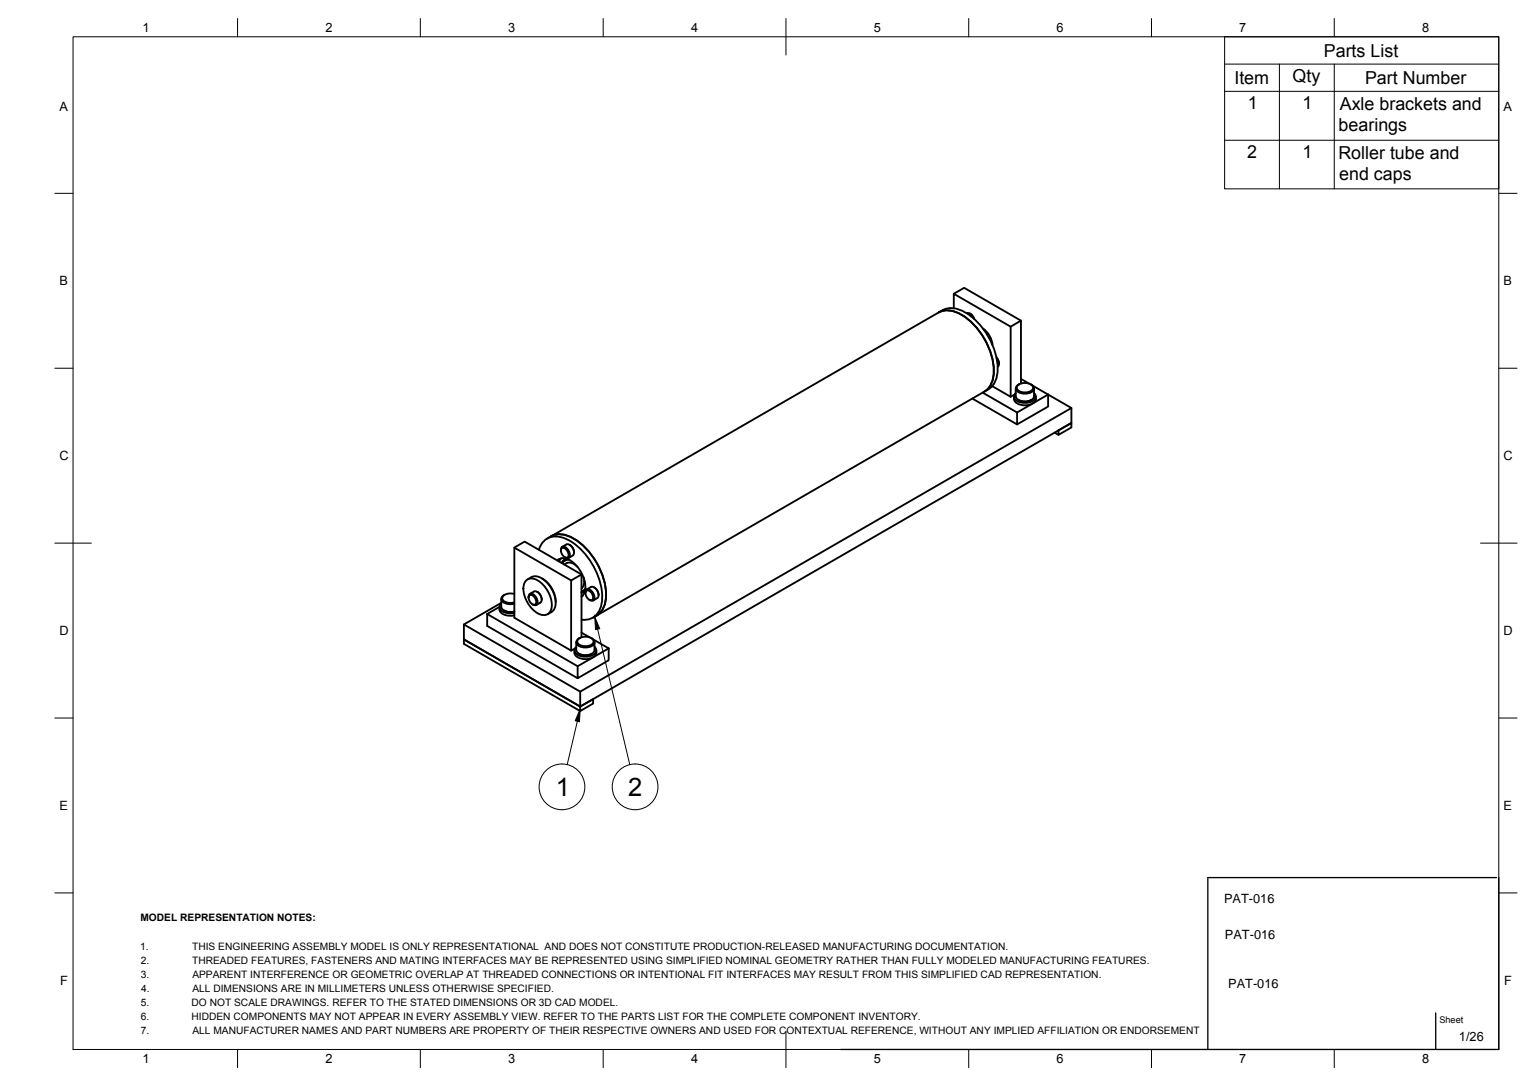
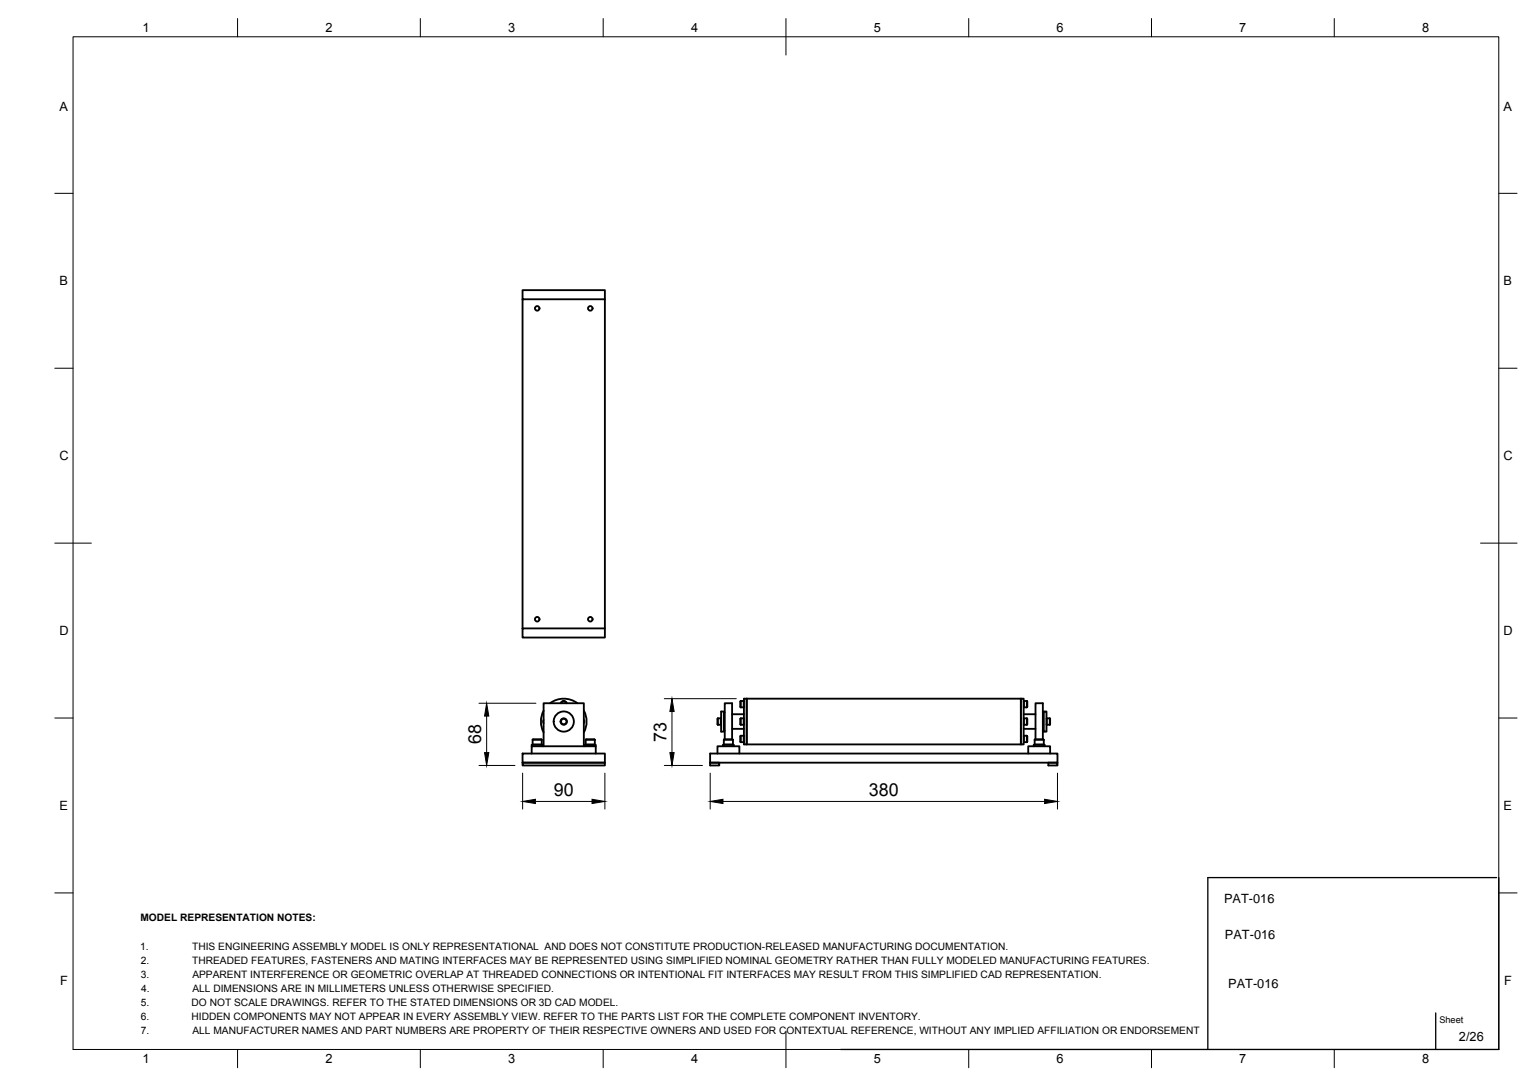
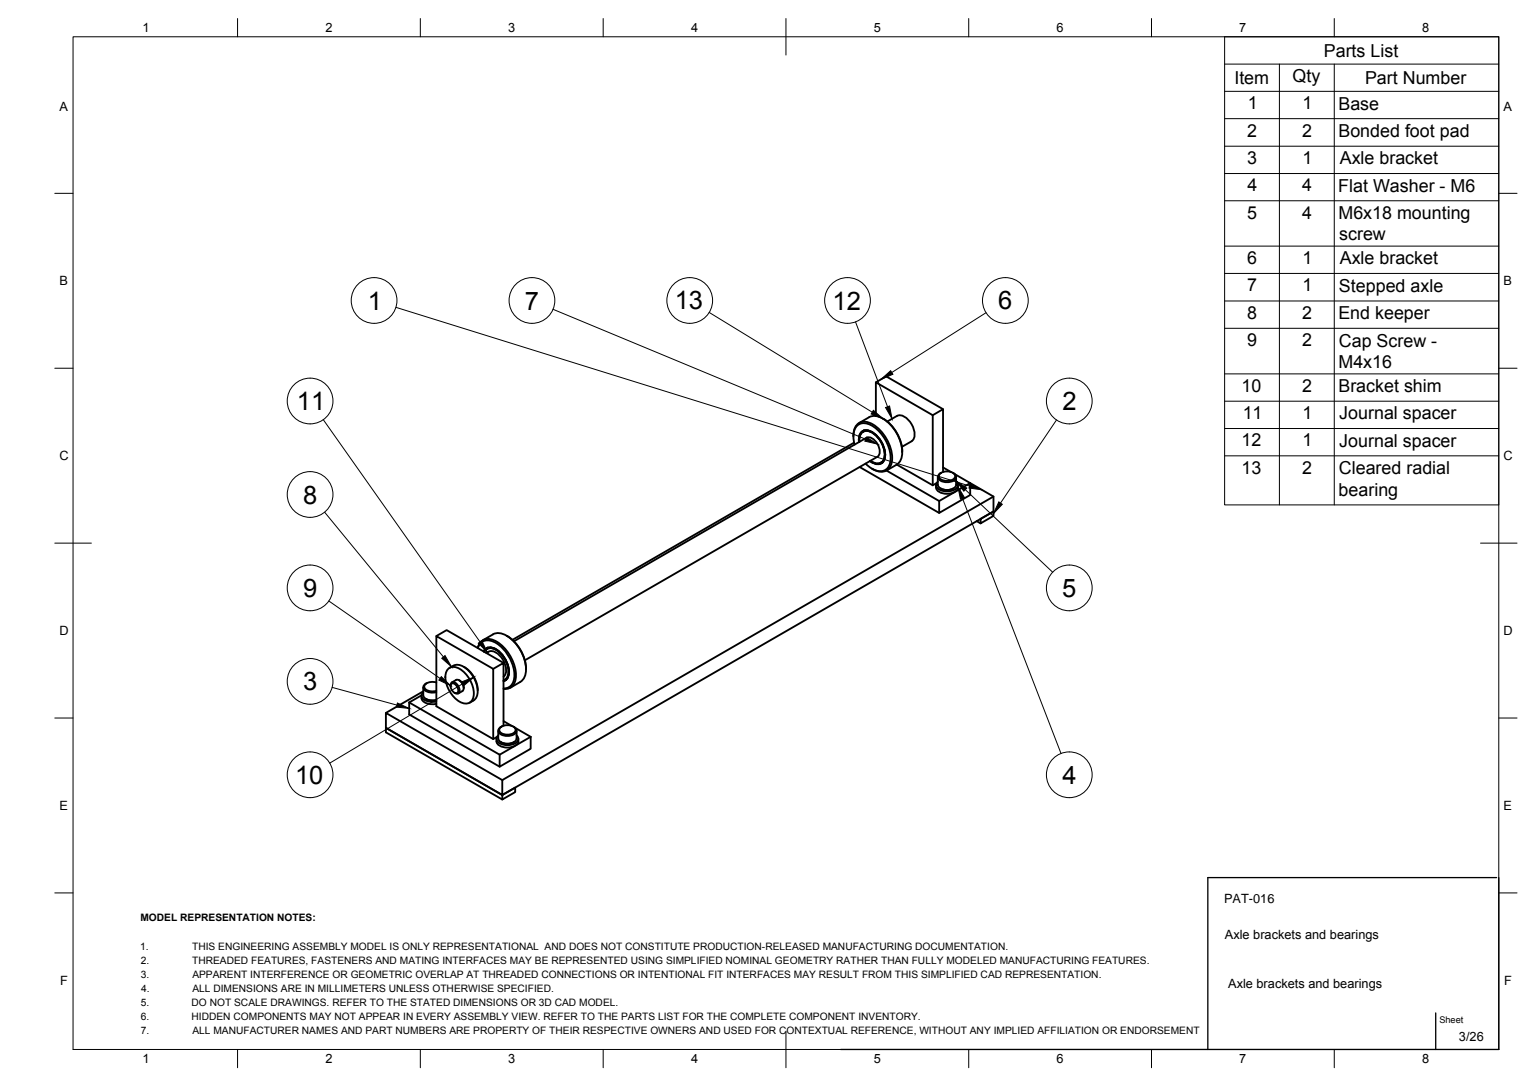
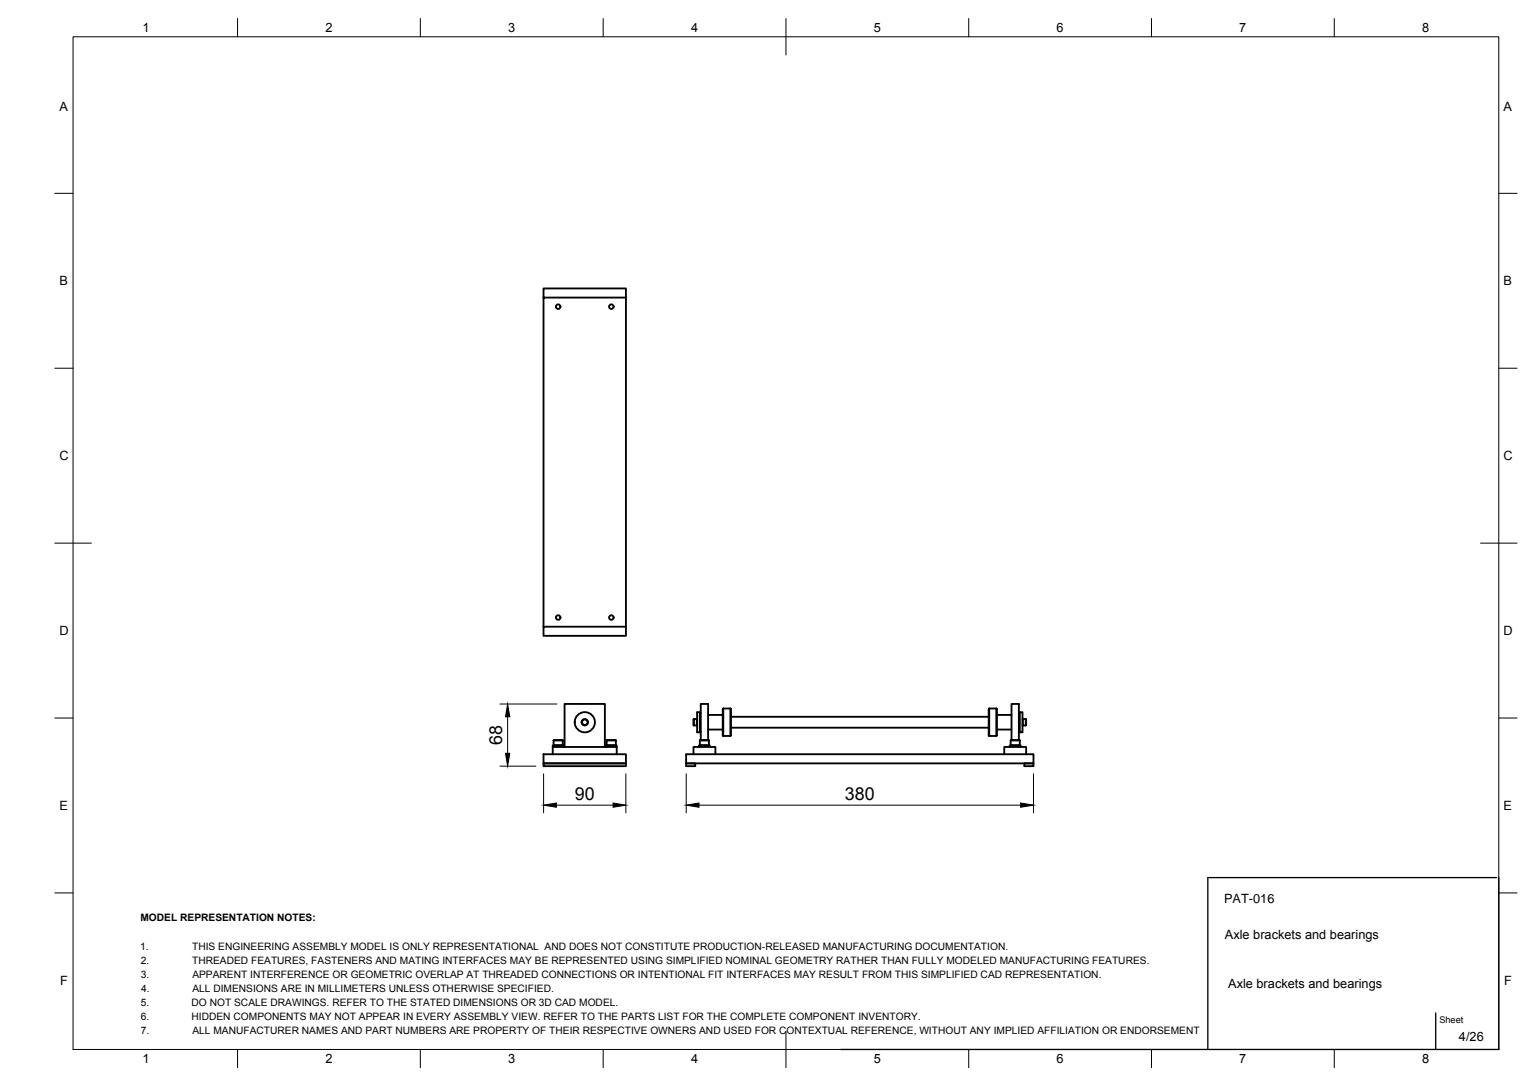
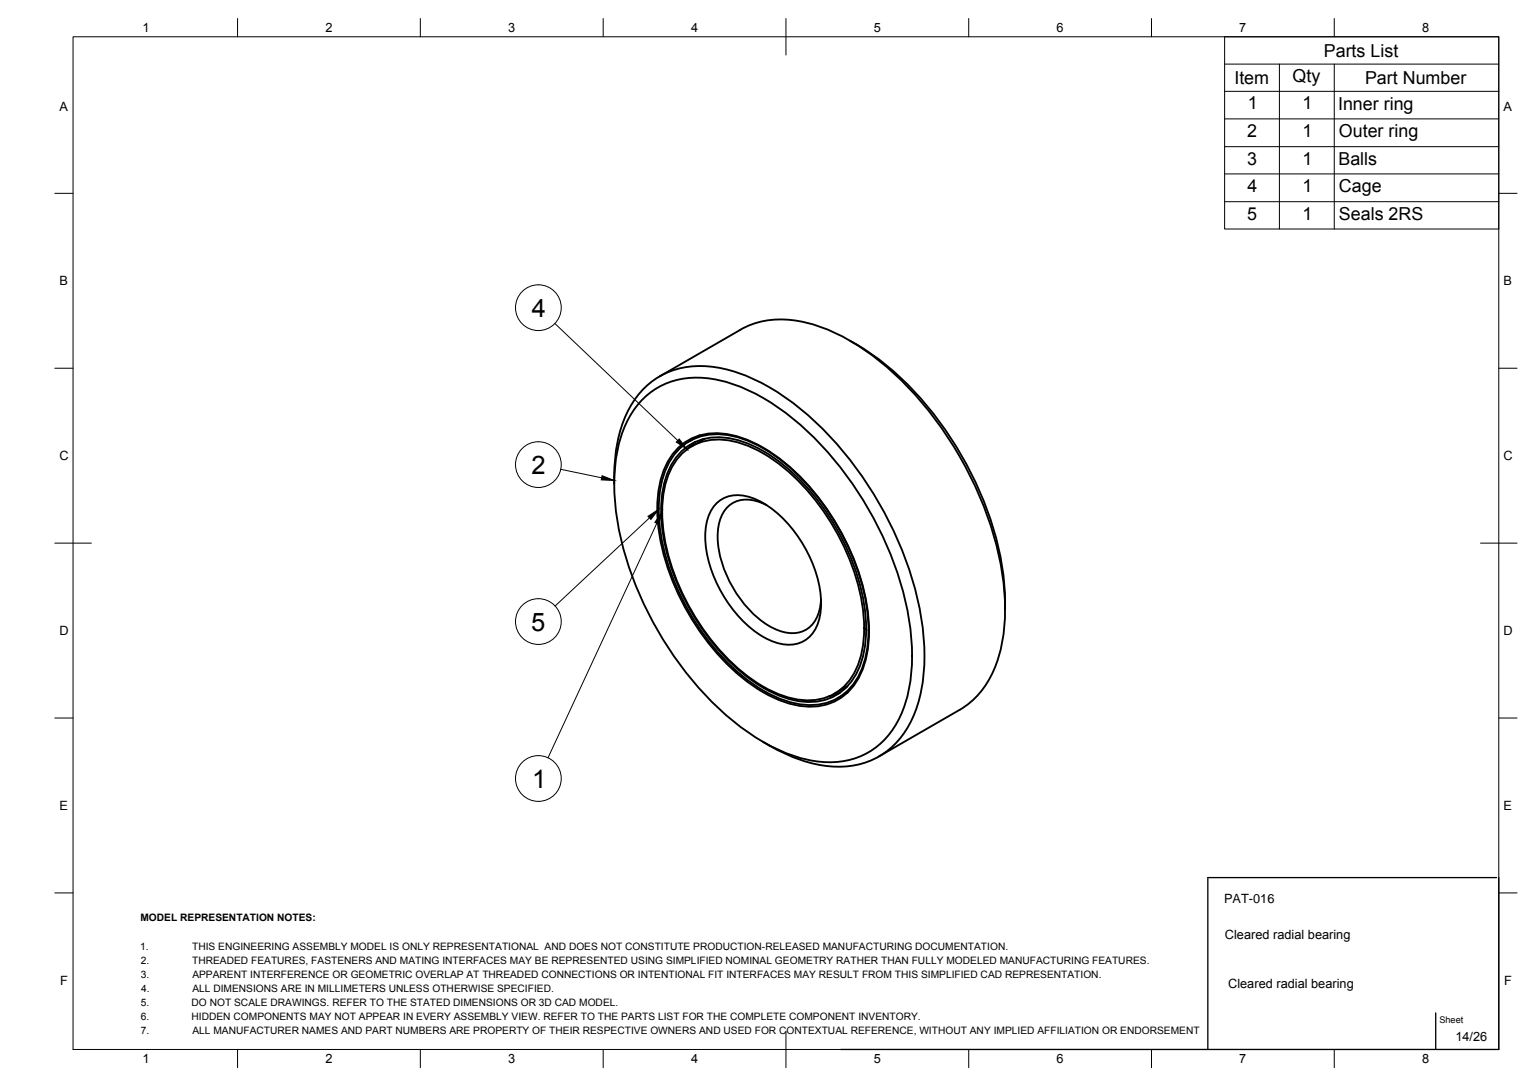
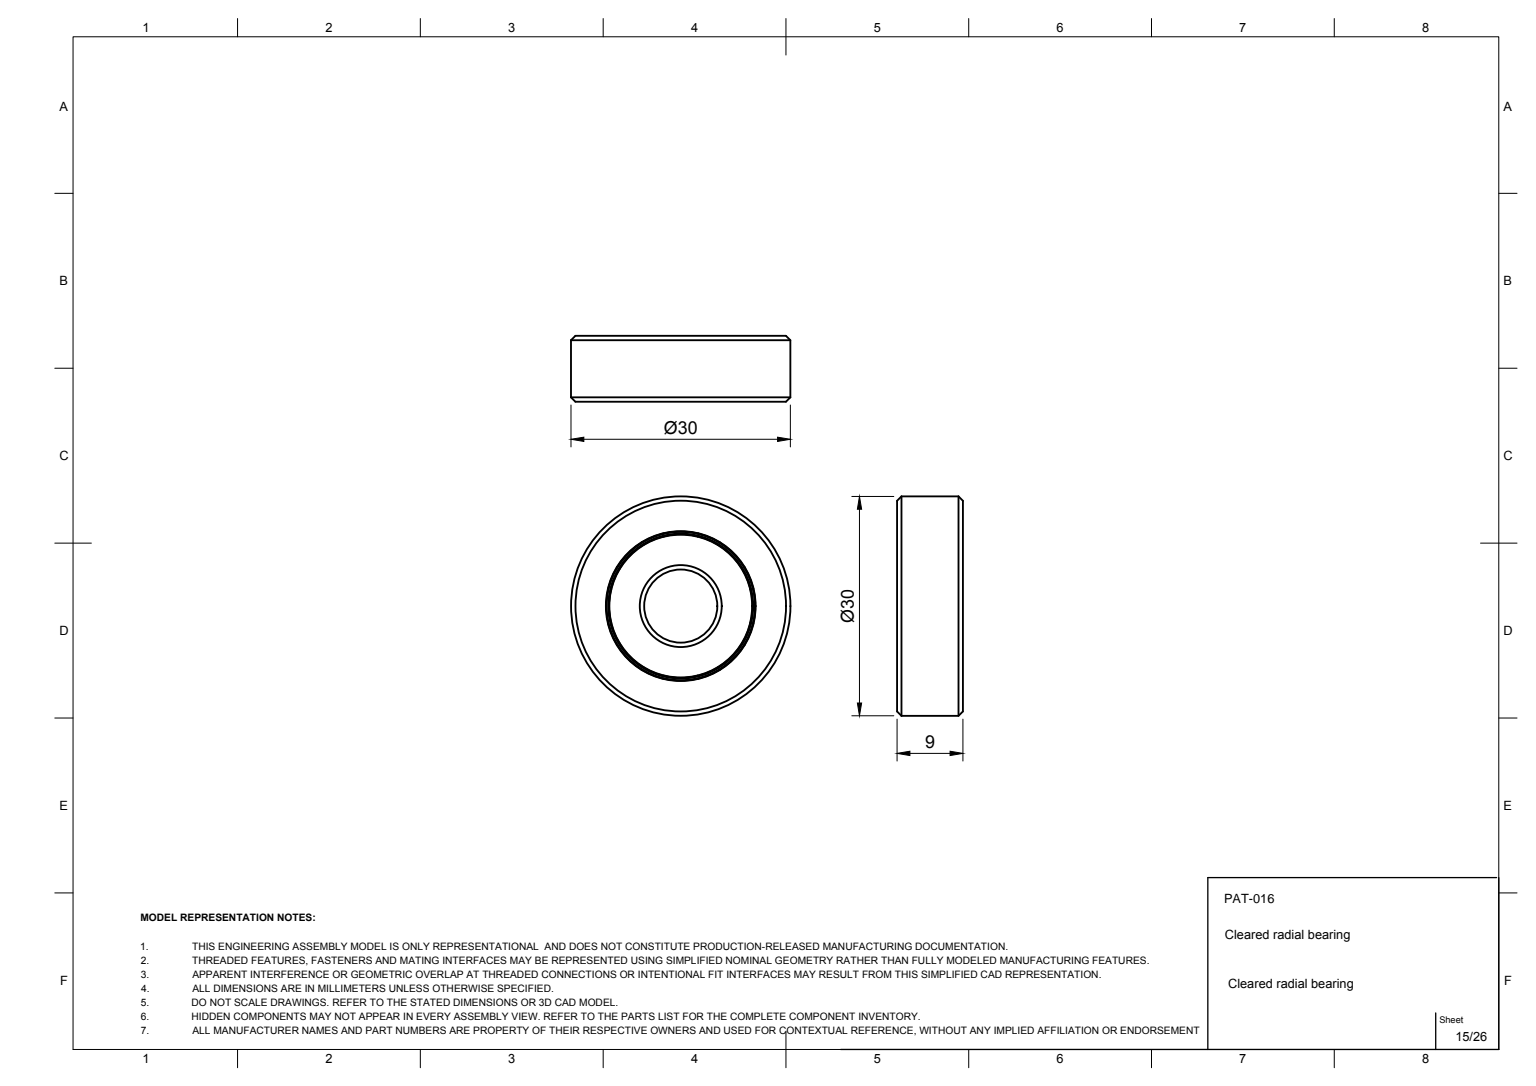
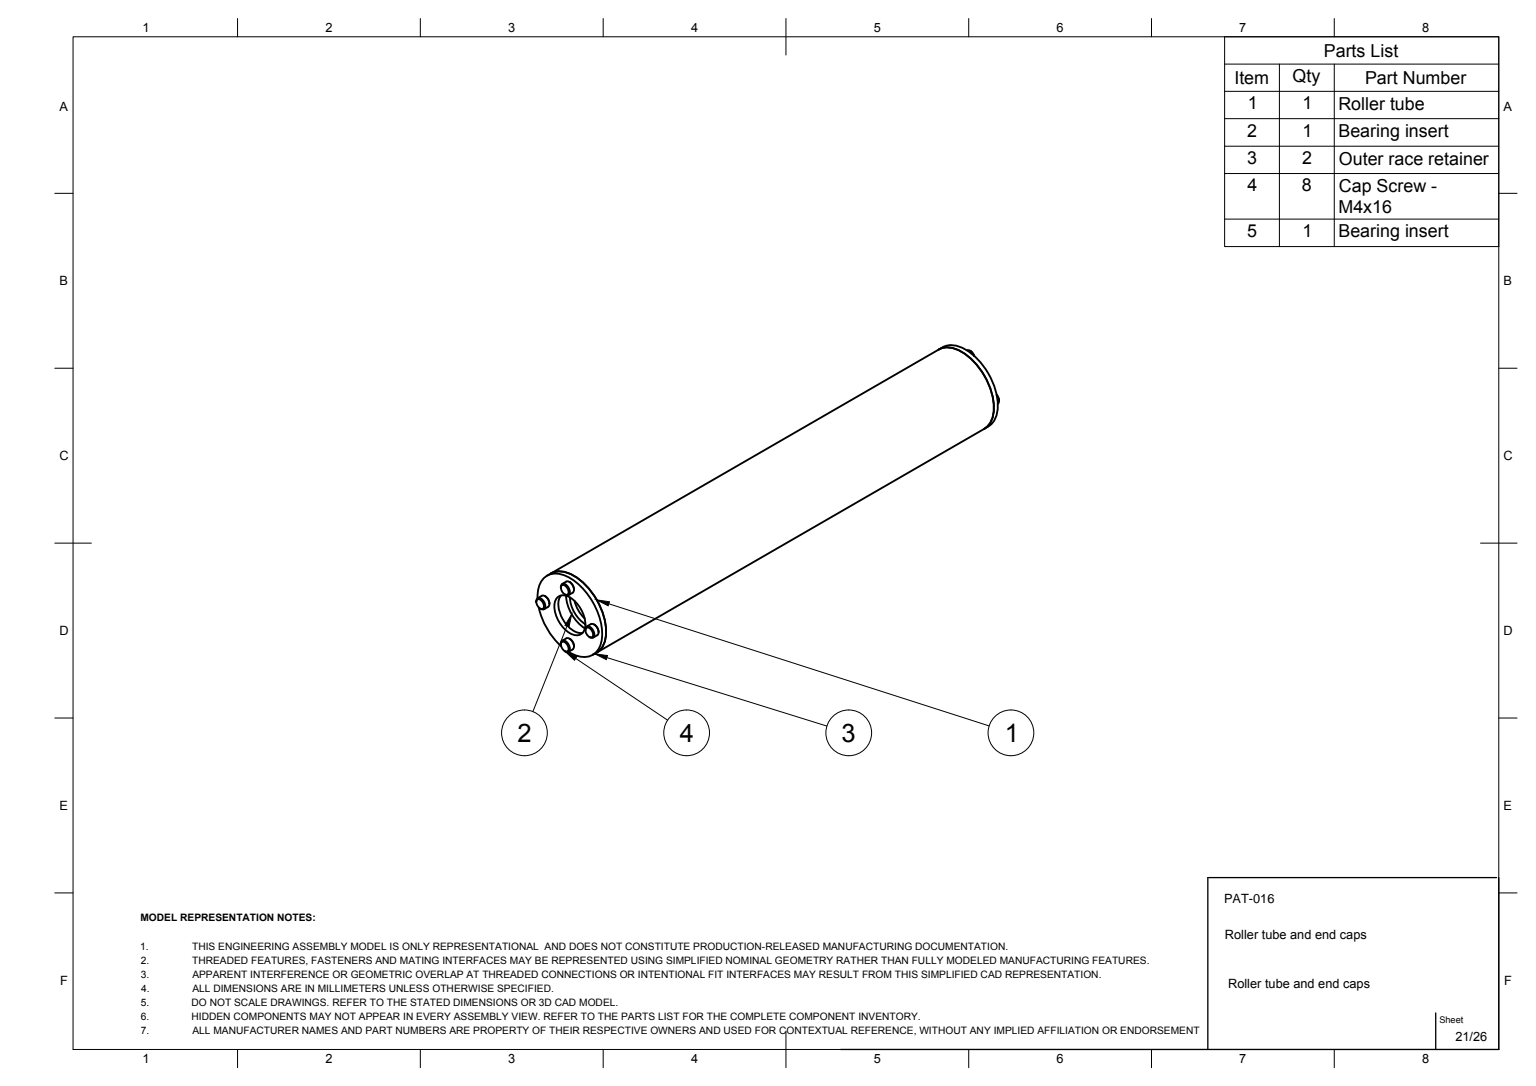
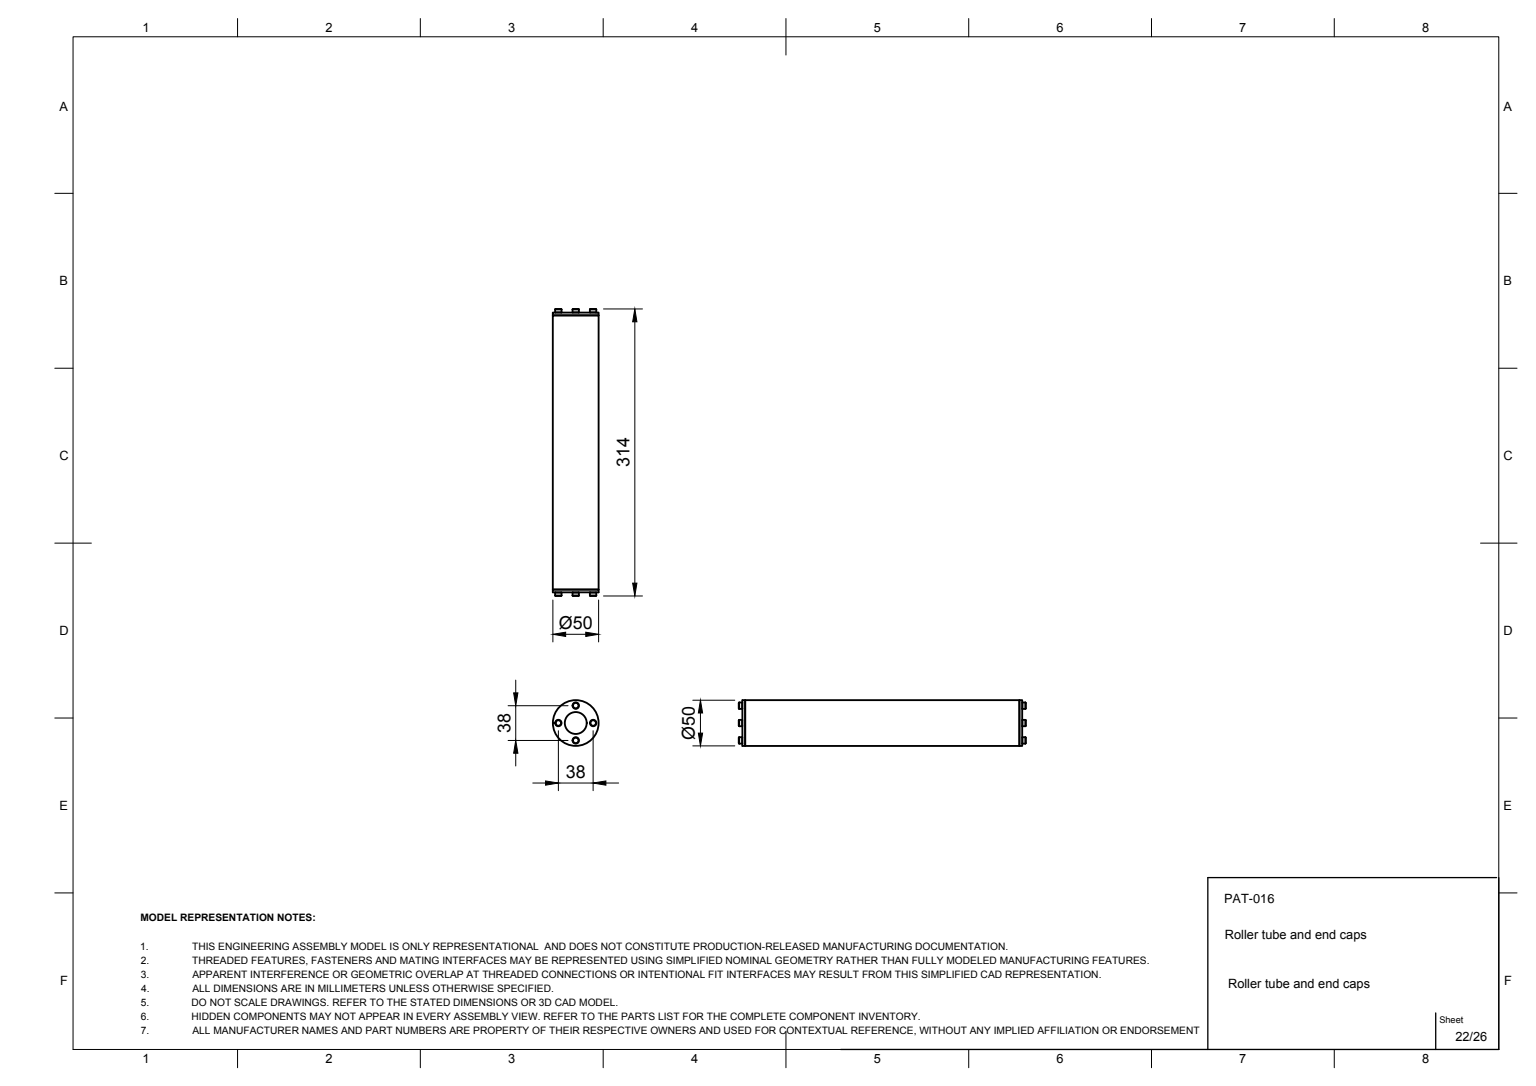
ISO-10303-21;
HEADER;
/* Generated by software containing ST-Developer
 * from STEP Tools, Inc. (www.steptools.com) 
 */

FILE_DESCRIPTION(
/* description */ ('Bracket-mounted idler roller'),
/* implementation_level */ '2;1');

FILE_NAME(
/* name */ 'PAT-016',
/* time_stamp */ '2026-10-28T03:26:42-07:00',
/* author */ (''),
/* organization */ (''),
/* preprocessor_version */ 'ST-DEVELOPER v20.2',
/* originating_system */ 'Autodesk Translation Framework v15.17.0.0',
/* authorisation */ '');

FILE_SCHEMA (('AUTOMOTIVE_DESIGN { 1 0 10303 214 3 1 1 }'));
ENDSEC;

DATA;
#10=MECHANICAL_DESIGN_GEOMETRIC_PRESENTATION_REPRESENTATION('',(#280,#281,
#282,#283,#284,#285,#286,#287,#288,#289,#290,#291,#292,#293,#294,#295,#296,
#297,#298,#299,#300,#301,#302,#303,#304,#305,#306,#307,#308),#6241);
#11=ITEM_DEFINED_TRANSFORMATION($,$,#3607,#3735);
#12=ITEM_DEFINED_TRANSFORMATION($,$,#3627,#3736);
#13=ITEM_DEFINED_TRANSFORMATION($,$,#3647,#3737);
#14=ITEM_DEFINED_TRANSFORMATION($,$,#3664,#3738);
#15=ITEM_DEFINED_TRANSFORMATION($,$,#3718,#3739);
#16=ITEM_DEFINED_TRANSFORMATION($,$,#3447,#3847);
#17=ITEM_DEFINED_TRANSFORMATION($,$,#3468,#3848);
#18=ITEM_DEFINED_TRANSFORMATION($,$,#3489,#3849);
#19=ITEM_DEFINED_TRANSFORMATION($,$,#3511,#3850);
#20=ITEM_DEFINED_TRANSFORMATION($,$,#3520,#3851);
#21=ITEM_DEFINED_TRANSFORMATION($,$,#3529,#3852);
#22=ITEM_DEFINED_TRANSFORMATION($,$,#3548,#3853);
#23=ITEM_DEFINED_TRANSFORMATION($,$,#3548,#3854);
#24=ITEM_DEFINED_TRANSFORMATION($,$,#3555,#3855);
#25=ITEM_DEFINED_TRANSFORMATION($,$,#3564,#3856);
#26=ITEM_DEFINED_TRANSFORMATION($,$,#3555,#3857);
#27=ITEM_DEFINED_TRANSFORMATION($,$,#3564,#3858);
#28=ITEM_DEFINED_TRANSFORMATION($,$,#3555,#3859);
#29=ITEM_DEFINED_TRANSFORMATION($,$,#3564,#3860);
#30=ITEM_DEFINED_TRANSFORMATION($,$,#3555,#3861);
#31=ITEM_DEFINED_TRANSFORMATION($,$,#3564,#3862);
#32=ITEM_DEFINED_TRANSFORMATION($,$,#3588,#3863);
#33=ITEM_DEFINED_TRANSFORMATION($,$,#3588,#3864);
#34=ITEM_DEFINED_TRANSFORMATION($,$,#3821,#3865);
#35=ITEM_DEFINED_TRANSFORMATION($,$,#3821,#3866);
#36=ITEM_DEFINED_TRANSFORMATION($,$,#3597,#3867);
#37=ITEM_DEFINED_TRANSFORMATION($,$,#3597,#3868);
#38=ITEM_DEFINED_TRANSFORMATION($,$,#3606,#3869);
#39=ITEM_DEFINED_TRANSFORMATION($,$,#3606,#3870);
#40=ITEM_DEFINED_TRANSFORMATION($,$,#3741,#3871);
#41=ITEM_DEFINED_TRANSFORMATION($,$,#3766,#3872);
#42=ITEM_DEFINED_TRANSFORMATION($,$,#3791,#3873);
#43=ITEM_DEFINED_TRANSFORMATION($,$,#3800,#3874);
#44=ITEM_DEFINED_TRANSFORMATION($,$,#3821,#3875);
#45=ITEM_DEFINED_TRANSFORMATION($,$,#3821,#3876);
#46=ITEM_DEFINED_TRANSFORMATION($,$,#3821,#3877);
#47=ITEM_DEFINED_TRANSFORMATION($,$,#3821,#3878);
#48=ITEM_DEFINED_TRANSFORMATION($,$,#3800,#3879);
#49=ITEM_DEFINED_TRANSFORMATION($,$,#3821,#3880);
#50=ITEM_DEFINED_TRANSFORMATION($,$,#3821,#3881);
#51=ITEM_DEFINED_TRANSFORMATION($,$,#3821,#3882);
#52=ITEM_DEFINED_TRANSFORMATION($,$,#3821,#3883);
#53=ITEM_DEFINED_TRANSFORMATION($,$,#3446,#3884);
#54=ITEM_DEFINED_TRANSFORMATION($,$,#3740,#3885);
#55=(
REPRESENTATION_RELATIONSHIP($,$,#6354,#6353)
REPRESENTATION_RELATIONSHIP_WITH_TRANSFORMATION(#11)
SHAPE_REPRESENTATION_RELATIONSHIP()
);
#56=(
REPRESENTATION_RELATIONSHIP($,$,#6355,#6353)
REPRESENTATION_RELATIONSHIP_WITH_TRANSFORMATION(#12)
SHAPE_REPRESENTATION_RELATIONSHIP()
);
#57=(
REPRESENTATION_RELATIONSHIP($,$,#6356,#6353)
REPRESENTATION_RELATIONSHIP_WITH_TRANSFORMATION(#13)
SHAPE_REPRESENTATION_RELATIONSHIP()
);
#58=(
REPRESENTATION_RELATIONSHIP($,$,#6357,#6353)
REPRESENTATION_RELATIONSHIP_WITH_TRANSFORMATION(#14)
SHAPE_REPRESENTATION_RELATIONSHIP()
);
#59=(
REPRESENTATION_RELATIONSHIP($,$,#6358,#6353)
REPRESENTATION_RELATIONSHIP_WITH_TRANSFORMATION(#15)
SHAPE_REPRESENTATION_RELATIONSHIP()
);
#60=(
REPRESENTATION_RELATIONSHIP($,$,#6342,#6341)
REPRESENTATION_RELATIONSHIP_WITH_TRANSFORMATION(#16)
SHAPE_REPRESENTATION_RELATIONSHIP()
);
#61=(
REPRESENTATION_RELATIONSHIP($,$,#6343,#6341)
REPRESENTATION_RELATIONSHIP_WITH_TRANSFORMATION(#17)
SHAPE_REPRESENTATION_RELATIONSHIP()
);
#62=(
REPRESENTATION_RELATIONSHIP($,$,#6344,#6341)
REPRESENTATION_RELATIONSHIP_WITH_TRANSFORMATION(#18)
SHAPE_REPRESENTATION_RELATIONSHIP()
);
#63=(
REPRESENTATION_RELATIONSHIP($,$,#6345,#6341)
REPRESENTATION_RELATIONSHIP_WITH_TRANSFORMATION(#19)
SHAPE_REPRESENTATION_RELATIONSHIP()
);
#64=(
REPRESENTATION_RELATIONSHIP($,$,#6346,#6341)
REPRESENTATION_RELATIONSHIP_WITH_TRANSFORMATION(#20)
SHAPE_REPRESENTATION_RELATIONSHIP()
);
#65=(
REPRESENTATION_RELATIONSHIP($,$,#6347,#6341)
REPRESENTATION_RELATIONSHIP_WITH_TRANSFORMATION(#21)
SHAPE_REPRESENTATION_RELATIONSHIP()
);
#66=(
REPRESENTATION_RELATIONSHIP($,$,#6348,#6341)
REPRESENTATION_RELATIONSHIP_WITH_TRANSFORMATION(#22)
SHAPE_REPRESENTATION_RELATIONSHIP()
);
#67=(
REPRESENTATION_RELATIONSHIP($,$,#6348,#6341)
REPRESENTATION_RELATIONSHIP_WITH_TRANSFORMATION(#23)
SHAPE_REPRESENTATION_RELATIONSHIP()
);
#68=(
REPRESENTATION_RELATIONSHIP($,$,#6349,#6341)
REPRESENTATION_RELATIONSHIP_WITH_TRANSFORMATION(#24)
SHAPE_REPRESENTATION_RELATIONSHIP()
);
#69=(
REPRESENTATION_RELATIONSHIP($,$,#6350,#6341)
REPRESENTATION_RELATIONSHIP_WITH_TRANSFORMATION(#25)
SHAPE_REPRESENTATION_RELATIONSHIP()
);
#70=(
REPRESENTATION_RELATIONSHIP($,$,#6349,#6341)
REPRESENTATION_RELATIONSHIP_WITH_TRANSFORMATION(#26)
SHAPE_REPRESENTATION_RELATIONSHIP()
);
#71=(
REPRESENTATION_RELATIONSHIP($,$,#6350,#6341)
REPRESENTATION_RELATIONSHIP_WITH_TRANSFORMATION(#27)
SHAPE_REPRESENTATION_RELATIONSHIP()
);
#72=(
REPRESENTATION_RELATIONSHIP($,$,#6349,#6341)
REPRESENTATION_RELATIONSHIP_WITH_TRANSFORMATION(#28)
SHAPE_REPRESENTATION_RELATIONSHIP()
);
#73=(
REPRESENTATION_RELATIONSHIP($,$,#6350,#6341)
REPRESENTATION_RELATIONSHIP_WITH_TRANSFORMATION(#29)
SHAPE_REPRESENTATION_RELATIONSHIP()
);
#74=(
REPRESENTATION_RELATIONSHIP($,$,#6349,#6341)
REPRESENTATION_RELATIONSHIP_WITH_TRANSFORMATION(#30)
SHAPE_REPRESENTATION_RELATIONSHIP()
);
#75=(
REPRESENTATION_RELATIONSHIP($,$,#6350,#6341)
REPRESENTATION_RELATIONSHIP_WITH_TRANSFORMATION(#31)
SHAPE_REPRESENTATION_RELATIONSHIP()
);
#76=(
REPRESENTATION_RELATIONSHIP($,$,#6351,#6341)
REPRESENTATION_RELATIONSHIP_WITH_TRANSFORMATION(#32)
SHAPE_REPRESENTATION_RELATIONSHIP()
);
#77=(
REPRESENTATION_RELATIONSHIP($,$,#6351,#6341)
REPRESENTATION_RELATIONSHIP_WITH_TRANSFORMATION(#33)
SHAPE_REPRESENTATION_RELATIONSHIP()
);
#78=(
REPRESENTATION_RELATIONSHIP($,$,#6364,#6341)
REPRESENTATION_RELATIONSHIP_WITH_TRANSFORMATION(#34)
SHAPE_REPRESENTATION_RELATIONSHIP()
);
#79=(
REPRESENTATION_RELATIONSHIP($,$,#6364,#6341)
REPRESENTATION_RELATIONSHIP_WITH_TRANSFORMATION(#35)
SHAPE_REPRESENTATION_RELATIONSHIP()
);
#80=(
REPRESENTATION_RELATIONSHIP($,$,#6352,#6341)
REPRESENTATION_RELATIONSHIP_WITH_TRANSFORMATION(#36)
SHAPE_REPRESENTATION_RELATIONSHIP()
);
#81=(
REPRESENTATION_RELATIONSHIP($,$,#6352,#6341)
REPRESENTATION_RELATIONSHIP_WITH_TRANSFORMATION(#37)
SHAPE_REPRESENTATION_RELATIONSHIP()
);
#82=(
REPRESENTATION_RELATIONSHIP($,$,#6353,#6341)
REPRESENTATION_RELATIONSHIP_WITH_TRANSFORMATION(#38)
SHAPE_REPRESENTATION_RELATIONSHIP()
);
#83=(
REPRESENTATION_RELATIONSHIP($,$,#6353,#6341)
REPRESENTATION_RELATIONSHIP_WITH_TRANSFORMATION(#39)
SHAPE_REPRESENTATION_RELATIONSHIP()
);
#84=(
REPRESENTATION_RELATIONSHIP($,$,#6360,#6359)
REPRESENTATION_RELATIONSHIP_WITH_TRANSFORMATION(#40)
SHAPE_REPRESENTATION_RELATIONSHIP()
);
#85=(
REPRESENTATION_RELATIONSHIP($,$,#6361,#6359)
REPRESENTATION_RELATIONSHIP_WITH_TRANSFORMATION(#41)
SHAPE_REPRESENTATION_RELATIONSHIP()
);
#86=(
REPRESENTATION_RELATIONSHIP($,$,#6362,#6359)
REPRESENTATION_RELATIONSHIP_WITH_TRANSFORMATION(#42)
SHAPE_REPRESENTATION_RELATIONSHIP()
);
#87=(
REPRESENTATION_RELATIONSHIP($,$,#6363,#6359)
REPRESENTATION_RELATIONSHIP_WITH_TRANSFORMATION(#43)
SHAPE_REPRESENTATION_RELATIONSHIP()
);
#88=(
REPRESENTATION_RELATIONSHIP($,$,#6364,#6359)
REPRESENTATION_RELATIONSHIP_WITH_TRANSFORMATION(#44)
SHAPE_REPRESENTATION_RELATIONSHIP()
);
#89=(
REPRESENTATION_RELATIONSHIP($,$,#6364,#6359)
REPRESENTATION_RELATIONSHIP_WITH_TRANSFORMATION(#45)
SHAPE_REPRESENTATION_RELATIONSHIP()
);
#90=(
REPRESENTATION_RELATIONSHIP($,$,#6364,#6359)
REPRESENTATION_RELATIONSHIP_WITH_TRANSFORMATION(#46)
SHAPE_REPRESENTATION_RELATIONSHIP()
);
#91=(
REPRESENTATION_RELATIONSHIP($,$,#6364,#6359)
REPRESENTATION_RELATIONSHIP_WITH_TRANSFORMATION(#47)
SHAPE_REPRESENTATION_RELATIONSHIP()
);
#92=(
REPRESENTATION_RELATIONSHIP($,$,#6363,#6359)
REPRESENTATION_RELATIONSHIP_WITH_TRANSFORMATION(#48)
SHAPE_REPRESENTATION_RELATIONSHIP()
);
#93=(
REPRESENTATION_RELATIONSHIP($,$,#6364,#6359)
REPRESENTATION_RELATIONSHIP_WITH_TRANSFORMATION(#49)
SHAPE_REPRESENTATION_RELATIONSHIP()
);
#94=(
REPRESENTATION_RELATIONSHIP($,$,#6364,#6359)
REPRESENTATION_RELATIONSHIP_WITH_TRANSFORMATION(#50)
SHAPE_REPRESENTATION_RELATIONSHIP()
);
#95=(
REPRESENTATION_RELATIONSHIP($,$,#6364,#6359)
REPRESENTATION_RELATIONSHIP_WITH_TRANSFORMATION(#51)
SHAPE_REPRESENTATION_RELATIONSHIP()
);
#96=(
REPRESENTATION_RELATIONSHIP($,$,#6364,#6359)
REPRESENTATION_RELATIONSHIP_WITH_TRANSFORMATION(#52)
SHAPE_REPRESENTATION_RELATIONSHIP()
);
#97=(
REPRESENTATION_RELATIONSHIP($,$,#6341,#6340)
REPRESENTATION_RELATIONSHIP_WITH_TRANSFORMATION(#53)
SHAPE_REPRESENTATION_RELATIONSHIP()
);
#98=(
REPRESENTATION_RELATIONSHIP($,$,#6359,#6340)
REPRESENTATION_RELATIONSHIP_WITH_TRANSFORMATION(#54)
SHAPE_REPRESENTATION_RELATIONSHIP()
);
#99=CONTEXT_DEPENDENT_SHAPE_REPRESENTATION(#55,#6290);
#100=CONTEXT_DEPENDENT_SHAPE_REPRESENTATION(#56,#6291);
#101=CONTEXT_DEPENDENT_SHAPE_REPRESENTATION(#57,#6292);
#102=CONTEXT_DEPENDENT_SHAPE_REPRESENTATION(#58,#6293);
#103=CONTEXT_DEPENDENT_SHAPE_REPRESENTATION(#59,#6294);
#104=CONTEXT_DEPENDENT_SHAPE_REPRESENTATION(#60,#6301);
#105=CONTEXT_DEPENDENT_SHAPE_REPRESENTATION(#61,#6302);
#106=CONTEXT_DEPENDENT_SHAPE_REPRESENTATION(#62,#6303);
#107=CONTEXT_DEPENDENT_SHAPE_REPRESENTATION(#63,#6304);
#108=CONTEXT_DEPENDENT_SHAPE_REPRESENTATION(#64,#6305);
#109=CONTEXT_DEPENDENT_SHAPE_REPRESENTATION(#65,#6306);
#110=CONTEXT_DEPENDENT_SHAPE_REPRESENTATION(#66,#6307);
#111=CONTEXT_DEPENDENT_SHAPE_REPRESENTATION(#67,#6308);
#112=CONTEXT_DEPENDENT_SHAPE_REPRESENTATION(#68,#6309);
#113=CONTEXT_DEPENDENT_SHAPE_REPRESENTATION(#69,#6310);
#114=CONTEXT_DEPENDENT_SHAPE_REPRESENTATION(#70,#6311);
#115=CONTEXT_DEPENDENT_SHAPE_REPRESENTATION(#71,#6312);
#116=CONTEXT_DEPENDENT_SHAPE_REPRESENTATION(#72,#6313);
#117=CONTEXT_DEPENDENT_SHAPE_REPRESENTATION(#73,#6314);
#118=CONTEXT_DEPENDENT_SHAPE_REPRESENTATION(#74,#6315);
#119=CONTEXT_DEPENDENT_SHAPE_REPRESENTATION(#75,#6316);
#120=CONTEXT_DEPENDENT_SHAPE_REPRESENTATION(#76,#6317);
#121=CONTEXT_DEPENDENT_SHAPE_REPRESENTATION(#77,#6318);
#122=CONTEXT_DEPENDENT_SHAPE_REPRESENTATION(#78,#6319);
#123=CONTEXT_DEPENDENT_SHAPE_REPRESENTATION(#79,#6320);
#124=CONTEXT_DEPENDENT_SHAPE_REPRESENTATION(#80,#6321);
#125=CONTEXT_DEPENDENT_SHAPE_REPRESENTATION(#81,#6322);
#126=CONTEXT_DEPENDENT_SHAPE_REPRESENTATION(#82,#6323);
#127=CONTEXT_DEPENDENT_SHAPE_REPRESENTATION(#83,#6324);
#128=CONTEXT_DEPENDENT_SHAPE_REPRESENTATION(#84,#6325);
#129=CONTEXT_DEPENDENT_SHAPE_REPRESENTATION(#85,#6326);
#130=CONTEXT_DEPENDENT_SHAPE_REPRESENTATION(#86,#6327);
#131=CONTEXT_DEPENDENT_SHAPE_REPRESENTATION(#87,#6328);
#132=CONTEXT_DEPENDENT_SHAPE_REPRESENTATION(#88,#6329);
#133=CONTEXT_DEPENDENT_SHAPE_REPRESENTATION(#89,#6330);
#134=CONTEXT_DEPENDENT_SHAPE_REPRESENTATION(#90,#6331);
#135=CONTEXT_DEPENDENT_SHAPE_REPRESENTATION(#91,#6332);
#136=CONTEXT_DEPENDENT_SHAPE_REPRESENTATION(#92,#6333);
#137=CONTEXT_DEPENDENT_SHAPE_REPRESENTATION(#93,#6334);
#138=CONTEXT_DEPENDENT_SHAPE_REPRESENTATION(#94,#6335);
#139=CONTEXT_DEPENDENT_SHAPE_REPRESENTATION(#95,#6336);
#140=CONTEXT_DEPENDENT_SHAPE_REPRESENTATION(#96,#6337);
#141=CONTEXT_DEPENDENT_SHAPE_REPRESENTATION(#97,#6338);
#142=CONTEXT_DEPENDENT_SHAPE_REPRESENTATION(#98,#6339);
#143=NEXT_ASSEMBLY_USAGE_OCCURRENCE('Inner ring:1','Inner ring:1',
'Inner ring:1',#6379,#6380,'Inner ring:1');
#144=NEXT_ASSEMBLY_USAGE_OCCURRENCE('Outer ring:1','Outer ring:1',
'Outer ring:1',#6379,#6381,'Outer ring:1');
#145=NEXT_ASSEMBLY_USAGE_OCCURRENCE('Balls:1','Balls:1','Balls:1',#6379,
#6382,'Balls:1');
#146=NEXT_ASSEMBLY_USAGE_OCCURRENCE('Cage:1','Cage:1','Cage:1',#6379,#6383,
'Cage:1');
#147=NEXT_ASSEMBLY_USAGE_OCCURRENCE('Seals 2RS:1','Seals 2RS:1',
'Seals 2RS:1',#6379,#6384,'Seals 2RS:1');
#148=NEXT_ASSEMBLY_USAGE_OCCURRENCE('Axle bracket:1','Axle bracket:1',
'Axle bracket:1',#6367,#6368,'Axle bracket:1');
#149=NEXT_ASSEMBLY_USAGE_OCCURRENCE('Axle bracket (1):1',
'Axle bracket (1):1','Axle bracket (1):1',#6367,#6369,
'Axle bracket (1):1');
#150=NEXT_ASSEMBLY_USAGE_OCCURRENCE('Stepped axle:1','Stepped axle:1',
'Stepped axle:1',#6367,#6370,'Stepped axle:1');
#151=NEXT_ASSEMBLY_USAGE_OCCURRENCE('Journal spacer:1',
'Journal spacer:1','Journal spacer:1',#6367,#6371,'Journal spacer:1');
#152=NEXT_ASSEMBLY_USAGE_OCCURRENCE('Journal spacer (1):1',
'Journal spacer (1):1','Journal spacer (1):1',#6367,#6372,
'Journal spacer (1):1');
#153=NEXT_ASSEMBLY_USAGE_OCCURRENCE('Base:2','Base:2','Base:2',#6367,#6373,
'Base:2');
#154=NEXT_ASSEMBLY_USAGE_OCCURRENCE('Bonded foot pad:2',
'Bonded foot pad:2','Bonded foot pad:2',#6367,#6374,'Bonded foot pad:2');
#155=NEXT_ASSEMBLY_USAGE_OCCURRENCE('Bonded foot pad:3',
'Bonded foot pad:3','Bonded foot pad:3',#6367,#6374,'Bonded foot pad:3');
#156=NEXT_ASSEMBLY_USAGE_OCCURRENCE('Flat Washer - M6:2',
'Flat Washer - M6:2','Flat Washer - M6:2',#6367,#6375,
'Flat Washer - M6:2');
#157=NEXT_ASSEMBLY_USAGE_OCCURRENCE('M6x18 mounting screw:2',
'M6x18 mounting screw:2','M6x18 mounting screw:2',#6367,#6376,
'M6x18 mounting screw:2');
#158=NEXT_ASSEMBLY_USAGE_OCCURRENCE('Flat Washer - M6:3',
'Flat Washer - M6:3','Flat Washer - M6:3',#6367,#6375,
'Flat Washer - M6:3');
#159=NEXT_ASSEMBLY_USAGE_OCCURRENCE('M6x18 mounting screw:3',
'M6x18 mounting screw:3','M6x18 mounting screw:3',#6367,#6376,
'M6x18 mounting screw:3');
#160=NEXT_ASSEMBLY_USAGE_OCCURRENCE('Flat Washer - M6:4',
'Flat Washer - M6:4','Flat Washer - M6:4',#6367,#6375,
'Flat Washer - M6:4');
#161=NEXT_ASSEMBLY_USAGE_OCCURRENCE('M6x18 mounting screw:4',
'M6x18 mounting screw:4','M6x18 mounting screw:4',#6367,#6376,
'M6x18 mounting screw:4');
#162=NEXT_ASSEMBLY_USAGE_OCCURRENCE('Flat Washer - M6:5',
'Flat Washer - M6:5','Flat Washer - M6:5',#6367,#6375,
'Flat Washer - M6:5');
#163=NEXT_ASSEMBLY_USAGE_OCCURRENCE('M6x18 mounting screw:5',
'M6x18 mounting screw:5','M6x18 mounting screw:5',#6367,#6376,
'M6x18 mounting screw:5');
#164=NEXT_ASSEMBLY_USAGE_OCCURRENCE('End keeper:2','End keeper:2',
'End keeper:2',#6367,#6377,'End keeper:2');
#165=NEXT_ASSEMBLY_USAGE_OCCURRENCE('End keeper:3','End keeper:3',
'End keeper:3',#6367,#6377,'End keeper:3');
#166=NEXT_ASSEMBLY_USAGE_OCCURRENCE('Cap Screw - M4x16:2',
'Cap Screw - M4x16:2','Cap Screw - M4x16:2',#6367,#6390,
'Cap Screw - M4x16:2');
#167=NEXT_ASSEMBLY_USAGE_OCCURRENCE('Cap Screw - M4x16:3',
'Cap Screw - M4x16:3','Cap Screw - M4x16:3',#6367,#6390,
'Cap Screw - M4x16:3');
#168=NEXT_ASSEMBLY_USAGE_OCCURRENCE('Bracket shim:2','Bracket shim:2',
'Bracket shim:2',#6367,#6378,'Bracket shim:2');
#169=NEXT_ASSEMBLY_USAGE_OCCURRENCE('Bracket shim:3','Bracket shim:3',
'Bracket shim:3',#6367,#6378,'Bracket shim:3');
#170=NEXT_ASSEMBLY_USAGE_OCCURRENCE('Cleared radial bearing:2',
'Cleared radial bearing:2','Cleared radial bearing:2',#6367,#6379,
'Cleared radial bearing:2');
#171=NEXT_ASSEMBLY_USAGE_OCCURRENCE('Cleared radial bearing:3',
'Cleared radial bearing:3','Cleared radial bearing:3',#6367,#6379,
'Cleared radial bearing:3');
#172=NEXT_ASSEMBLY_USAGE_OCCURRENCE('Bearing insert:1',
'Bearing insert:1','Bearing insert:1',#6385,#6386,'Bearing insert:1');
#173=NEXT_ASSEMBLY_USAGE_OCCURRENCE('Bearing insert (1):1',
'Bearing insert (1):1','Bearing insert (1):1',#6385,#6387,
'Bearing insert (1):1');
#174=NEXT_ASSEMBLY_USAGE_OCCURRENCE('Roller tube:2','Roller tube:2',
'Roller tube:2',#6385,#6388,'Roller tube:2');
#175=NEXT_ASSEMBLY_USAGE_OCCURRENCE('Outer race retainer:2',
'Outer race retainer:2','Outer race retainer:2',#6385,#6389,
'Outer race retainer:2');
#176=NEXT_ASSEMBLY_USAGE_OCCURRENCE('Cap Screw - M4x16:4',
'Cap Screw - M4x16:4','Cap Screw - M4x16:4',#6385,#6390,
'Cap Screw - M4x16:4');
#177=NEXT_ASSEMBLY_USAGE_OCCURRENCE('Cap Screw - M4x16:5',
'Cap Screw - M4x16:5','Cap Screw - M4x16:5',#6385,#6390,
'Cap Screw - M4x16:5');
#178=NEXT_ASSEMBLY_USAGE_OCCURRENCE('Cap Screw - M4x16:6',
'Cap Screw - M4x16:6','Cap Screw - M4x16:6',#6385,#6390,
'Cap Screw - M4x16:6');
#179=NEXT_ASSEMBLY_USAGE_OCCURRENCE('Cap Screw - M4x16:7',
'Cap Screw - M4x16:7','Cap Screw - M4x16:7',#6385,#6390,
'Cap Screw - M4x16:7');
#180=NEXT_ASSEMBLY_USAGE_OCCURRENCE('Outer race retainer:3',
'Outer race retainer:3','Outer race retainer:3',#6385,#6389,
'Outer race retainer:3');
#181=NEXT_ASSEMBLY_USAGE_OCCURRENCE('Cap Screw - M4x16:8',
'Cap Screw - M4x16:8','Cap Screw - M4x16:8',#6385,#6390,
'Cap Screw - M4x16:8');
#182=NEXT_ASSEMBLY_USAGE_OCCURRENCE('Cap Screw - M4x16:9',
'Cap Screw - M4x16:9','Cap Screw - M4x16:9',#6385,#6390,
'Cap Screw - M4x16:9');
#183=NEXT_ASSEMBLY_USAGE_OCCURRENCE('Cap Screw - M4x16:10',
'Cap Screw - M4x16:10','Cap Screw - M4x16:10',#6385,#6390,
'Cap Screw - M4x16:10');
#184=NEXT_ASSEMBLY_USAGE_OCCURRENCE('Cap Screw - M4x16:11',
'Cap Screw - M4x16:11','Cap Screw - M4x16:11',#6385,#6390,
'Cap Screw - M4x16:11');
#185=NEXT_ASSEMBLY_USAGE_OCCURRENCE('Axle brackets and bearings:1',
'Axle brackets and bearings:1','Axle brackets and bearings:1',#6366,#6367,
'Axle brackets and bearings:1');
#186=NEXT_ASSEMBLY_USAGE_OCCURRENCE('Roller tube and end caps:1',
'Roller tube and end caps:1','Roller tube and end caps:1',#6366,#6385,
'Roller tube and end caps:1');
#187=B_SPLINE_CURVE_WITH_KNOTS('',3,(#5456,#5457,#5458,#5459,#5460,#5461,
#5462,#5463,#5464,#5465,#5466,#5467,#5468,#5469,#5470,#5471,#5472,#5473,
#5474,#5475,#5476,#5477),.UNSPECIFIED.,.F.,.F.,(4,2,2,2,2,2,2,2,2,2,4),
(0.0473477652366656,0.126350602536658,0.189525903804987,0.252701205073317,
0.313298422430275,0.373895639787233,0.434492857144191,0.495090074501149,
0.558265375769478,0.621440677037807,0.7004435143378),.UNSPECIFIED.);
#188=B_SPLINE_CURVE_WITH_KNOTS('',3,(#5481,#5482,#5483,#5484,#5485,#5486,
#5487,#5488,#5489,#5490,#5491,#5492,#5493,#5494,#5495,#5496,#5497,#5498,
#5499,#5500,#5501,#5502),.UNSPECIFIED.,.F.,.F.,(4,2,2,2,2,2,2,2,2,2,4),
(0.0464897534940957,0.0852567806515119,0.170513561303024,0.246687263103517,
0.308657850341199,0.370628437578881,0.432599024816563,0.494569612054245,
0.570743313854739,0.656000094506251,0.694767121663666),.UNSPECIFIED.);
#189=B_SPLINE_CURVE_WITH_KNOTS('',3,(#5508,#5509,#5510,#5511,#5512,#5513,
#5514,#5515,#5516,#5517,#5518,#5519,#5520,#5521,#5522,#5523,#5524,#5525,
#5526,#5527,#5528,#5529),.UNSPECIFIED.,.F.,.F.,(4,2,2,2,2,2,2,2,2,2,4),
(0.0464897534940957,0.0852567806515118,0.170513561303024,0.246687263103517,
0.308657850341199,0.370628437578881,0.432599024816563,0.494569612054245,
0.570743313854738,0.65600009450625,0.694767121663666),.UNSPECIFIED.);
#190=B_SPLINE_CURVE_WITH_KNOTS('',3,(#5533,#5534,#5535,#5536,#5537,#5538,
#5539,#5540,#5541,#5542,#5543,#5544,#5545,#5546,#5547,#5548,#5549,#5550,
#5551,#5552,#5553,#5554),.UNSPECIFIED.,.F.,.F.,(4,2,2,2,2,2,2,2,2,2,4),
(0.0464897534940957,0.0852567806515119,0.170513561303024,0.246687263103517,
0.308657850341199,0.370628437578881,0.432599024816563,0.494569612054245,
0.570743313854739,0.656000094506251,0.694767121663666),.UNSPECIFIED.);
#191=B_SPLINE_CURVE_WITH_KNOTS('',3,(#5558,#5559,#5560,#5561,#5562,#5563,
#5564,#5565,#5566,#5567,#5568,#5569),.UNSPECIFIED.,.F.,.F.,(4,2,2,2,2,4),
(0.0464897534940957,0.0852567806515119,0.170513561303024,0.246687263103517,
0.308657850341199,0.370628437578881),.UNSPECIFIED.);
#192=B_SPLINE_CURVE_WITH_KNOTS('',3,(#5574,#5575,#5576,#5577,#5578,#5579,
#5580,#5581,#5582,#5583,#5584,#5585),.UNSPECIFIED.,.F.,.F.,(4,2,2,2,2,4),
(0.370628437578881,0.432599024816563,0.494569612054245,0.570743313854738,
0.65600009450625,0.694767121663666),.UNSPECIFIED.);
#193=B_SPLINE_CURVE_WITH_KNOTS('',3,(#5589,#5590,#5591,#5592,#5593,#5594,
#5595,#5596,#5597,#5598,#5599,#5600,#5601,#5602,#5603,#5604,#5605,#5606,
#5607,#5608,#5609,#5610),.UNSPECIFIED.,.F.,.F.,(4,2,2,2,2,2,2,2,2,2,4),
(0.0464897534940957,0.0852567806515121,0.170513561303024,0.246687263103518,
0.308657850341199,0.370628437578881,0.432599024816563,0.494569612054245,
0.570743313854738,0.65600009450625,0.694767121663666),.UNSPECIFIED.);
#194=B_SPLINE_CURVE_WITH_KNOTS('',3,(#5614,#5615,#5616,#5617,#5618,#5619,
#5620,#5621,#5622,#5623,#5624,#5625,#5626,#5627,#5628,#5629,#5630,#5631,
#5632,#5633,#5634,#5635),.UNSPECIFIED.,.F.,.F.,(4,2,2,2,2,2,2,2,2,2,4),
(0.0464897534940957,0.0852567806515119,0.170513561303024,0.246687263103517,
0.308657850341199,0.370628437578881,0.432599024816563,0.494569612054245,
0.570743313854738,0.65600009450625,0.694767121663667),.UNSPECIFIED.);
#195=B_SPLINE_CURVE_WITH_KNOTS('',3,(#5639,#5640,#5641,#5642,#5643,#5644,
#5645,#5646,#5647,#5648,#5649,#5650,#5651,#5652,#5653,#5654,#5655,#5656,
#5657,#5658,#5659,#5660),.UNSPECIFIED.,.F.,.F.,(4,2,2,2,2,2,2,2,2,2,4),
(0.0464897534940957,0.0852567806515119,0.170513561303024,0.246687263103517,
0.308657850341199,0.370628437578881,0.432599024816563,0.494569612054245,
0.570743313854738,0.65600009450625,0.694767121663666),.UNSPECIFIED.);
#196=B_SPLINE_CURVE_WITH_KNOTS('',3,(#5664,#5665,#5666,#5667,#5668,#5669,
#5670,#5671,#5672,#5673,#5674,#5675,#5676,#5677,#5678,#5679,#5680,#5681,
#5682,#5683,#5684,#5685),.UNSPECIFIED.,.F.,.F.,(4,2,2,2,2,2,2,2,2,2,4),
(0.0464897534940957,0.0852567806515119,0.170513561303024,0.246687263103517,
0.308657850341199,0.370628437578881,0.432599024816563,0.494569612054245,
0.570743313854739,0.656000094506251,0.694767121663667),.UNSPECIFIED.);
#197=B_SPLINE_CURVE_WITH_KNOTS('',3,(#5693,#5694,#5695,#5696,#5697,#5698,
#5699,#5700,#5701,#5702,#5703,#5704,#5705,#5706,#5707,#5708,#5709,#5710,
#5711,#5712,#5713,#5714),.UNSPECIFIED.,.F.,.F.,(4,2,2,2,2,2,2,2,2,2,4),
(0.0473477652366656,0.126350602536658,0.189525903804987,0.252701205073316,
0.313298422430274,0.373895639787232,0.434492857144191,0.495090074501149,
0.558265375769478,0.621440677037807,0.7004435143378),.UNSPECIFIED.);
#198=B_SPLINE_CURVE_WITH_KNOTS('',3,(#5722,#5723,#5724,#5725,#5726,#5727,
#5728,#5729,#5730,#5731,#5732,#5733,#5734,#5735,#5736,#5737,#5738,#5739,
#5740,#5741,#5742,#5743),.UNSPECIFIED.,.F.,.F.,(4,2,2,2,2,2,2,2,2,2,4),
(0.0473477652366656,0.126350602536658,0.189525903804987,0.252701205073317,
0.313298422430275,0.373895639787233,0.434492857144191,0.495090074501149,
0.558265375769478,0.621440677037807,0.7004435143378),.UNSPECIFIED.);
#199=B_SPLINE_CURVE_WITH_KNOTS('',3,(#5752,#5753,#5754,#5755,#5756,#5757,
#5758,#5759,#5760,#5761,#5762,#5763),.UNSPECIFIED.,.F.,.F.,(4,2,2,2,2,4),
(0.0473477652366656,0.126350602536658,0.189525903804987,0.252701205073316,
0.313298422430275,0.373895639787233),.UNSPECIFIED.);
#200=B_SPLINE_CURVE_WITH_KNOTS('',3,(#5765,#5766,#5767,#5768,#5769,#5770,
#5771,#5772,#5773,#5774,#5775,#5776),.UNSPECIFIED.,.F.,.F.,(4,2,2,2,2,4),
(0.373895639787233,0.434492857144191,0.495090074501149,0.558265375769478,
0.621440677037807,0.7004435143378),.UNSPECIFIED.);
#201=B_SPLINE_CURVE_WITH_KNOTS('',3,(#5783,#5784,#5785,#5786,#5787,#5788,
#5789,#5790,#5791,#5792,#5793,#5794,#5795,#5796,#5797,#5798,#5799,#5800,
#5801,#5802,#5803,#5804),.UNSPECIFIED.,.F.,.F.,(4,2,2,2,2,2,2,2,2,2,4),
(0.0473477652366656,0.126350602536658,0.189525903804987,0.252701205073316,
0.313298422430275,0.373895639787233,0.434492857144191,0.495090074501149,
0.558265375769478,0.621440677037807,0.7004435143378),.UNSPECIFIED.);
#202=B_SPLINE_CURVE_WITH_KNOTS('',3,(#5812,#5813,#5814,#5815,#5816,#5817,
#5818,#5819,#5820,#5821,#5822,#5823,#5824,#5825,#5826,#5827,#5828,#5829,
#5830,#5831,#5832,#5833),.UNSPECIFIED.,.F.,.F.,(4,2,2,2,2,2,2,2,2,2,4),
(0.0473477652366656,0.126350602536658,0.189525903804987,0.252701205073317,
0.313298422430275,0.373895639787233,0.434492857144191,0.495090074501149,
0.558265375769478,0.621440677037807,0.7004435143378),.UNSPECIFIED.);
#203=B_SPLINE_CURVE_WITH_KNOTS('',3,(#5841,#5842,#5843,#5844,#5845,#5846,
#5847,#5848,#5849,#5850,#5851,#5852,#5853,#5854,#5855,#5856,#5857,#5858,
#5859,#5860,#5861,#5862),.UNSPECIFIED.,.F.,.F.,(4,2,2,2,2,2,2,2,2,2,4),
(0.0473477652366656,0.126350602536658,0.189525903804987,0.252701205073316,
0.313298422430275,0.373895639787233,0.434492857144191,0.495090074501149,
0.558265375769478,0.621440677037807,0.7004435143378),.UNSPECIFIED.);
#204=B_SPLINE_CURVE_WITH_KNOTS('',3,(#5871,#5872,#5873,#5874,#5875,#5876,
#5877,#5878,#5879,#5880,#5881,#5882,#5883,#5884,#5885,#5886,#5887,#5888,
#5889,#5890,#5891,#5892),.UNSPECIFIED.,.F.,.F.,(4,2,2,2,2,2,2,2,2,2,4),
(0.0473477652366656,0.126350602536658,0.189525903804987,0.252701205073317,
0.313298422430275,0.373895639787233,0.434492857144191,0.495090074501149,
0.558265375769478,0.621440677037807,0.7004435143378),.UNSPECIFIED.);
#205=SPHERICAL_SURFACE('',#3648,0.23815);
#206=SPHERICAL_SURFACE('',#3650,0.23815);
#207=SPHERICAL_SURFACE('',#3652,0.23815);
#208=SPHERICAL_SURFACE('',#3654,0.23815);
#209=SPHERICAL_SURFACE('',#3656,0.23815);
#210=SPHERICAL_SURFACE('',#3658,0.23815);
#211=SPHERICAL_SURFACE('',#3660,0.23815);
#212=SPHERICAL_SURFACE('',#3662,0.23815);
#213=SPHERICAL_SURFACE('',#3665,0.247676);
#214=SPHERICAL_SURFACE('',#3681,0.247676);
#215=SPHERICAL_SURFACE('',#3686,0.247676);
#216=SPHERICAL_SURFACE('',#3691,0.247676);
#217=SPHERICAL_SURFACE('',#3696,0.247676);
#218=SPHERICAL_SURFACE('',#3701,0.247676);
#219=SPHERICAL_SURFACE('',#3706,0.247676);
#220=SPHERICAL_SURFACE('',#3714,0.247676);
#221=TOROIDAL_SURFACE('',#3608,1.,0.247676);
#222=TOROIDAL_SURFACE('',#3628,1.,0.247676);
#223=CONICAL_SURFACE('',#3577,0.475,0.785398163397449);
#224=CONICAL_SURFACE('',#3581,0.485,0.785398163397448);
#225=CONICAL_SURFACE('',#3585,0.31,0.463647609000806);
#226=CONICAL_SURFACE('',#3619,0.53,0.785398163397448);
#227=CONICAL_SURFACE('',#3626,0.53,0.785398163397448);
#228=CONICAL_SURFACE('',#3639,1.47,0.785398163397449);
#229=CONICAL_SURFACE('',#3643,1.47,0.785398163397449);
#230=CONICAL_SURFACE('',#3824,0.325,0.785398163397448);
#231=CONICAL_SURFACE('',#3828,0.335,0.785398163397448);
#232=CONICAL_SURFACE('',#3832,0.21,0.463647609000806);
#233=CONICAL_SURFACE('',#3836,0.18,0.785398163397448);
#234=ORIENTED_CLOSED_SHELL('',*,#3190,.F.);
#235=ORIENTED_CLOSED_SHELL('',*,#3212,.F.);
#236=BREP_WITH_VOIDS('Body1',#3191,(#234));
#237=BREP_WITH_VOIDS('Body1',#3211,(#235));
#238=SHAPE_REPRESENTATION_RELATIONSHIP('SRR','None',#6342,#259);
#239=SHAPE_REPRESENTATION_RELATIONSHIP('SRR','None',#6343,#260);
#240=SHAPE_REPRESENTATION_RELATIONSHIP('SRR','None',#6344,#261);
#241=SHAPE_REPRESENTATION_RELATIONSHIP('SRR','None',#6345,#262);
#242=SHAPE_REPRESENTATION_RELATIONSHIP('SRR','None',#6346,#263);
#243=SHAPE_REPRESENTATION_RELATIONSHIP('SRR','None',#6347,#264);
#244=SHAPE_REPRESENTATION_RELATIONSHIP('SRR','None',#6348,#265);
#245=SHAPE_REPRESENTATION_RELATIONSHIP('SRR','None',#6349,#266);
#246=SHAPE_REPRESENTATION_RELATIONSHIP('SRR','None',#6350,#267);
#247=SHAPE_REPRESENTATION_RELATIONSHIP('SRR','None',#6351,#268);
#248=SHAPE_REPRESENTATION_RELATIONSHIP('SRR','None',#6352,#269);
#249=SHAPE_REPRESENTATION_RELATIONSHIP('SRR','None',#6354,#270);
#250=SHAPE_REPRESENTATION_RELATIONSHIP('SRR','None',#6355,#271);
#251=SHAPE_REPRESENTATION_RELATIONSHIP('SRR','None',#6356,#272);
#252=SHAPE_REPRESENTATION_RELATIONSHIP('SRR','None',#6357,#273);
#253=SHAPE_REPRESENTATION_RELATIONSHIP('SRR','None',#6358,#274);
#254=SHAPE_REPRESENTATION_RELATIONSHIP('SRR','None',#6360,#275);
#255=SHAPE_REPRESENTATION_RELATIONSHIP('SRR','None',#6361,#276);
#256=SHAPE_REPRESENTATION_RELATIONSHIP('SRR','None',#6362,#277);
#257=SHAPE_REPRESENTATION_RELATIONSHIP('SRR','None',#6363,#278);
#258=SHAPE_REPRESENTATION_RELATIONSHIP('SRR','None',#6364,#279);
#259=ADVANCED_BREP_SHAPE_REPRESENTATION('',(#309),#6218);
#260=ADVANCED_BREP_SHAPE_REPRESENTATION('',(#310),#6219);
#261=ADVANCED_BREP_SHAPE_REPRESENTATION('',(#311),#6220);
#262=ADVANCED_BREP_SHAPE_REPRESENTATION('',(#312),#6221);
#263=ADVANCED_BREP_SHAPE_REPRESENTATION('',(#313),#6222);
#264=ADVANCED_BREP_SHAPE_REPRESENTATION('',(#314),#6223);
#265=ADVANCED_BREP_SHAPE_REPRESENTATION('',(#315),#6224);
#266=ADVANCED_BREP_SHAPE_REPRESENTATION('',(#316),#6225);
#267=ADVANCED_BREP_SHAPE_REPRESENTATION('',(#236),#6226);
#268=ADVANCED_BREP_SHAPE_REPRESENTATION('',(#317),#6227);
#269=ADVANCED_BREP_SHAPE_REPRESENTATION('',(#318),#6228);
#270=ADVANCED_BREP_SHAPE_REPRESENTATION('',(#319),#6230);
#271=ADVANCED_BREP_SHAPE_REPRESENTATION('',(#320),#6231);
#272=ADVANCED_BREP_SHAPE_REPRESENTATION('',(#321,#322,#323,#324,#325,#326,
#327,#328),#6232);
#273=ADVANCED_BREP_SHAPE_REPRESENTATION('',(#329),#6233);
#274=ADVANCED_BREP_SHAPE_REPRESENTATION('',(#330,#331),#6234);
#275=ADVANCED_BREP_SHAPE_REPRESENTATION('',(#332),#6236);
#276=ADVANCED_BREP_SHAPE_REPRESENTATION('',(#333),#6237);
#277=ADVANCED_BREP_SHAPE_REPRESENTATION('',(#334),#6238);
#278=ADVANCED_BREP_SHAPE_REPRESENTATION('',(#335),#6239);
#279=ADVANCED_BREP_SHAPE_REPRESENTATION('',(#237),#6240);
#280=STYLED_ITEM('',(#6538),#309);
#281=STYLED_ITEM('',(#6538),#310);
#282=STYLED_ITEM('',(#6538),#311);
#283=STYLED_ITEM('',(#6531),#312);
#284=STYLED_ITEM('',(#6531),#313);
#285=STYLED_ITEM('',(#6517),#314);
#286=STYLED_ITEM('',(#6531),#315);
#287=STYLED_ITEM('',(#6545),#316);
#288=STYLED_ITEM('',(#6545),#236);
#289=STYLED_ITEM('',(#6552),#317);
#290=STYLED_ITEM('',(#6517),#318);
#291=STYLED_ITEM('',(#6538),#319);
#292=STYLED_ITEM('',(#6538),#320);
#293=STYLED_ITEM('',(#6538),#321);
#294=STYLED_ITEM('',(#6538),#322);
#295=STYLED_ITEM('',(#6538),#323);
#296=STYLED_ITEM('',(#6538),#324);
#297=STYLED_ITEM('',(#6538),#325);
#298=STYLED_ITEM('',(#6538),#326);
#299=STYLED_ITEM('',(#6538),#327);
#300=STYLED_ITEM('',(#6538),#328);
#301=STYLED_ITEM('',(#6538),#329);
#302=STYLED_ITEM('',(#6538),#330);
#303=STYLED_ITEM('',(#6538),#331);
#304=STYLED_ITEM('',(#6538),#332);
#305=STYLED_ITEM('',(#6538),#333);
#306=STYLED_ITEM('',(#6524),#334);
#307=STYLED_ITEM('',(#6538),#335);
#308=STYLED_ITEM('',(#6545),#237);
#309=MANIFOLD_SOLID_BREP('Body1',#3182);
#310=MANIFOLD_SOLID_BREP('Body1',#3183);
#311=MANIFOLD_SOLID_BREP('Body1',#3184);
#312=MANIFOLD_SOLID_BREP('Body1',#3185);
#313=MANIFOLD_SOLID_BREP('Body1',#3186);
#314=MANIFOLD_SOLID_BREP('Body1',#3187);
#315=MANIFOLD_SOLID_BREP('Body1',#3188);
#316=MANIFOLD_SOLID_BREP('Body1',#3189);
#317=MANIFOLD_SOLID_BREP('Body1',#3192);
#318=MANIFOLD_SOLID_BREP('Body1',#3193);
#319=MANIFOLD_SOLID_BREP('Body1',#3194);
#320=MANIFOLD_SOLID_BREP('Body1',#3195);
#321=MANIFOLD_SOLID_BREP('Body1',#3196);
#322=MANIFOLD_SOLID_BREP('Body2',#3197);
#323=MANIFOLD_SOLID_BREP('Body3',#3198);
#324=MANIFOLD_SOLID_BREP('Body4',#3199);
#325=MANIFOLD_SOLID_BREP('Body5',#3200);
#326=MANIFOLD_SOLID_BREP('Body6',#3201);
#327=MANIFOLD_SOLID_BREP('Body7',#3202);
#328=MANIFOLD_SOLID_BREP('Body8',#3203);
#329=MANIFOLD_SOLID_BREP('Continuous crown cage',#3204);
#330=MANIFOLD_SOLID_BREP('Body1',#3205);
#331=MANIFOLD_SOLID_BREP('Body2',#3206);
#332=MANIFOLD_SOLID_BREP('Body1',#3207);
#333=MANIFOLD_SOLID_BREP('Body1',#3208);
#334=MANIFOLD_SOLID_BREP('Body1',#3209);
#335=MANIFOLD_SOLID_BREP('Body1',#3210);
#336=FACE_BOUND('',#711,.T.);
#337=FACE_BOUND('',#712,.T.);
#338=FACE_BOUND('',#713,.T.);
#339=FACE_BOUND('',#719,.T.);
#340=FACE_BOUND('',#722,.T.);
#341=FACE_BOUND('',#726,.T.);
#342=FACE_BOUND('',#727,.T.);
#343=FACE_BOUND('',#732,.T.);
#344=FACE_BOUND('',#733,.T.);
#345=FACE_BOUND('',#734,.T.);
#346=FACE_BOUND('',#740,.T.);
#347=FACE_BOUND('',#743,.T.);
#348=FACE_BOUND('',#747,.T.);
#349=FACE_BOUND('',#748,.T.);
#350=FACE_BOUND('',#754,.T.);
#351=FACE_BOUND('',#756,.T.);
#352=FACE_BOUND('',#761,.T.);
#353=FACE_BOUND('',#763,.T.);
#354=FACE_BOUND('',#767,.T.);
#355=FACE_BOUND('',#769,.T.);
#356=FACE_BOUND('',#773,.T.);
#357=FACE_BOUND('',#775,.T.);
#358=FACE_BOUND('',#785,.T.);
#359=FACE_BOUND('',#786,.T.);
#360=FACE_BOUND('',#787,.T.);
#361=FACE_BOUND('',#788,.T.);
#362=FACE_BOUND('',#790,.T.);
#363=FACE_BOUND('',#791,.T.);
#364=FACE_BOUND('',#792,.T.);
#365=FACE_BOUND('',#793,.T.);
#366=FACE_BOUND('',#803,.T.);
#367=FACE_BOUND('',#805,.T.);
#368=FACE_BOUND('',#820,.T.);
#369=FACE_BOUND('',#826,.T.);
#370=FACE_BOUND('',#828,.T.);
#371=FACE_BOUND('',#832,.T.);
#372=FACE_BOUND('',#834,.T.);
#373=FACE_BOUND('',#840,.T.);
#374=FACE_BOUND('',#843,.T.);
#375=FACE_BOUND('',#848,.T.);
#376=FACE_BOUND('',#853,.T.);
#377=FACE_BOUND('',#881,.T.);
#378=FACE_BOUND('',#884,.T.);
#379=FACE_BOUND('',#887,.T.);
#380=FACE_BOUND('',#890,.T.);
#381=FACE_BOUND('',#893,.T.);
#382=FACE_BOUND('',#901,.T.);
#383=FACE_BOUND('',#905,.T.);
#384=FACE_BOUND('',#906,.T.);
#385=FACE_BOUND('',#907,.T.);
#386=FACE_BOUND('',#908,.T.);
#387=FACE_BOUND('',#909,.T.);
#388=FACE_BOUND('',#911,.T.);
#389=FACE_BOUND('',#912,.T.);
#390=FACE_BOUND('',#913,.T.);
#391=FACE_BOUND('',#914,.T.);
#392=FACE_BOUND('',#915,.T.);
#393=FACE_BOUND('',#922,.T.);
#394=FACE_BOUND('',#926,.T.);
#395=FACE_BOUND('',#927,.T.);
#396=FACE_BOUND('',#928,.T.);
#397=FACE_BOUND('',#929,.T.);
#398=FACE_BOUND('',#930,.T.);
#399=FACE_BOUND('',#932,.T.);
#400=FACE_BOUND('',#933,.T.);
#401=FACE_BOUND('',#934,.T.);
#402=FACE_BOUND('',#935,.T.);
#403=FACE_BOUND('',#936,.T.);
#404=FACE_BOUND('',#940,.T.);
#405=FACE_BOUND('',#942,.T.);
#406=FACE_BOUND('',#950,.T.);
#407=FACE_BOUND('',#951,.T.);
#408=FACE_BOUND('',#952,.T.);
#409=FACE_BOUND('',#953,.T.);
#410=FACE_BOUND('',#954,.T.);
#411=FACE_BOUND('',#956,.T.);
#412=FACE_BOUND('',#957,.T.);
#413=FACE_BOUND('',#958,.T.);
#414=FACE_BOUND('',#959,.T.);
#415=FACE_BOUND('',#960,.T.);
#416=FACE_BOUND('',#966,.T.);
#417=PLANE('',#3457);
#418=PLANE('',#3458);
#419=PLANE('',#3459);
#420=PLANE('',#3460);
#421=PLANE('',#3461);
#422=PLANE('',#3462);
#423=PLANE('',#3463);
#424=PLANE('',#3464);
#425=PLANE('',#3465);
#426=PLANE('',#3466);
#427=PLANE('',#3467);
#428=PLANE('',#3478);
#429=PLANE('',#3479);
#430=PLANE('',#3480);
#431=PLANE('',#3481);
#432=PLANE('',#3482);
#433=PLANE('',#3483);
#434=PLANE('',#3484);
#435=PLANE('',#3485);
#436=PLANE('',#3486);
#437=PLANE('',#3487);
#438=PLANE('',#3488);
#439=PLANE('',#3493);
#440=PLANE('',#3497);
#441=PLANE('',#3498);
#442=PLANE('',#3501);
#443=PLANE('',#3509);
#444=PLANE('',#3510);
#445=PLANE('',#3518);
#446=PLANE('',#3519);
#447=PLANE('',#3527);
#448=PLANE('',#3528);
#449=PLANE('',#3542);
#450=PLANE('',#3543);
#451=PLANE('',#3544);
#452=PLANE('',#3545);
#453=PLANE('',#3546);
#454=PLANE('',#3547);
#455=PLANE('',#3549);
#456=PLANE('',#3550);
#457=PLANE('',#3551);
#458=PLANE('',#3552);
#459=PLANE('',#3553);
#460=PLANE('',#3554);
#461=PLANE('',#3562);
#462=PLANE('',#3563);
#463=PLANE('',#3565);
#464=PLANE('',#3566);
#465=PLANE('',#3567);
#466=PLANE('',#3568);
#467=PLANE('',#3569);
#468=PLANE('',#3570);
#469=PLANE('',#3571);
#470=PLANE('',#3572);
#471=PLANE('',#3573);
#472=PLANE('',#3575);
#473=PLANE('',#3583);
#474=PLANE('',#3595);
#475=PLANE('',#3596);
#476=PLANE('',#3604);
#477=PLANE('',#3605);
#478=PLANE('',#3621);
#479=PLANE('',#3624);
#480=PLANE('',#3636);
#481=PLANE('',#3645);
#482=PLANE('',#3678);
#483=PLANE('',#3683);
#484=PLANE('',#3688);
#485=PLANE('',#3693);
#486=PLANE('',#3698);
#487=PLANE('',#3703);
#488=PLANE('',#3712);
#489=PLANE('',#3716);
#490=PLANE('',#3717);
#491=PLANE('',#3719);
#492=PLANE('',#3724);
#493=PLANE('',#3727);
#494=PLANE('',#3732);
#495=PLANE('',#3757);
#496=PLANE('',#3764);
#497=PLANE('',#3765);
#498=PLANE('',#3782);
#499=PLANE('',#3789);
#500=PLANE('',#3790);
#501=PLANE('',#3798);
#502=PLANE('',#3799);
#503=PLANE('',#3819);
#504=PLANE('',#3820);
#505=PLANE('',#3822);
#506=PLANE('',#3830);
#507=PLANE('',#3838);
#508=PLANE('',#3839);
#509=PLANE('',#3840);
#510=PLANE('',#3841);
#511=PLANE('',#3842);
#512=PLANE('',#3843);
#513=PLANE('',#3844);
#514=PLANE('',#3845);
#515=PLANE('',#3846);
#516=FACE_OUTER_BOUND('',#707,.T.);
#517=FACE_OUTER_BOUND('',#708,.T.);
#518=FACE_OUTER_BOUND('',#709,.T.);
#519=FACE_OUTER_BOUND('',#710,.T.);
#520=FACE_OUTER_BOUND('',#714,.T.);
#521=FACE_OUTER_BOUND('',#715,.T.);
#522=FACE_OUTER_BOUND('',#716,.T.);
#523=FACE_OUTER_BOUND('',#717,.T.);
#524=FACE_OUTER_BOUND('',#718,.T.);
#525=FACE_OUTER_BOUND('',#720,.T.);
#526=FACE_OUTER_BOUND('',#721,.T.);
#527=FACE_OUTER_BOUND('',#723,.T.);
#528=FACE_OUTER_BOUND('',#724,.T.);
#529=FACE_OUTER_BOUND('',#725,.T.);
#530=FACE_OUTER_BOUND('',#728,.T.);
#531=FACE_OUTER_BOUND('',#729,.T.);
#532=FACE_OUTER_BOUND('',#730,.T.);
#533=FACE_OUTER_BOUND('',#731,.T.);
#534=FACE_OUTER_BOUND('',#735,.T.);
#535=FACE_OUTER_BOUND('',#736,.T.);
#536=FACE_OUTER_BOUND('',#737,.T.);
#537=FACE_OUTER_BOUND('',#738,.T.);
#538=FACE_OUTER_BOUND('',#739,.T.);
#539=FACE_OUTER_BOUND('',#741,.T.);
#540=FACE_OUTER_BOUND('',#742,.T.);
#541=FACE_OUTER_BOUND('',#744,.T.);
#542=FACE_OUTER_BOUND('',#745,.T.);
#543=FACE_OUTER_BOUND('',#746,.T.);
#544=FACE_OUTER_BOUND('',#749,.T.);
#545=FACE_OUTER_BOUND('',#750,.T.);
#546=FACE_OUTER_BOUND('',#751,.T.);
#547=FACE_OUTER_BOUND('',#752,.T.);
#548=FACE_OUTER_BOUND('',#753,.T.);
#549=FACE_OUTER_BOUND('',#755,.T.);
#550=FACE_OUTER_BOUND('',#757,.T.);
#551=FACE_OUTER_BOUND('',#758,.T.);
#552=FACE_OUTER_BOUND('',#759,.T.);
#553=FACE_OUTER_BOUND('',#760,.T.);
#554=FACE_OUTER_BOUND('',#762,.T.);
#555=FACE_OUTER_BOUND('',#764,.T.);
#556=FACE_OUTER_BOUND('',#765,.T.);
#557=FACE_OUTER_BOUND('',#766,.T.);
#558=FACE_OUTER_BOUND('',#768,.T.);
#559=FACE_OUTER_BOUND('',#770,.T.);
#560=FACE_OUTER_BOUND('',#771,.T.);
#561=FACE_OUTER_BOUND('',#772,.T.);
#562=FACE_OUTER_BOUND('',#774,.T.);
#563=FACE_OUTER_BOUND('',#776,.T.);
#564=FACE_OUTER_BOUND('',#777,.T.);
#565=FACE_OUTER_BOUND('',#778,.T.);
#566=FACE_OUTER_BOUND('',#779,.T.);
#567=FACE_OUTER_BOUND('',#780,.T.);
#568=FACE_OUTER_BOUND('',#781,.T.);
#569=FACE_OUTER_BOUND('',#782,.T.);
#570=FACE_OUTER_BOUND('',#783,.T.);
#571=FACE_OUTER_BOUND('',#784,.T.);
#572=FACE_OUTER_BOUND('',#789,.T.);
#573=FACE_OUTER_BOUND('',#794,.T.);
#574=FACE_OUTER_BOUND('',#795,.T.);
#575=FACE_OUTER_BOUND('',#796,.T.);
#576=FACE_OUTER_BOUND('',#797,.T.);
#577=FACE_OUTER_BOUND('',#798,.T.);
#578=FACE_OUTER_BOUND('',#799,.T.);
#579=FACE_OUTER_BOUND('',#800,.T.);
#580=FACE_OUTER_BOUND('',#801,.T.);
#581=FACE_OUTER_BOUND('',#802,.T.);
#582=FACE_OUTER_BOUND('',#804,.T.);
#583=FACE_OUTER_BOUND('',#806,.T.);
#584=FACE_OUTER_BOUND('',#807,.T.);
#585=FACE_OUTER_BOUND('',#808,.T.);
#586=FACE_OUTER_BOUND('',#809,.T.);
#587=FACE_OUTER_BOUND('',#810,.T.);
#588=FACE_OUTER_BOUND('',#811,.T.);
#589=FACE_OUTER_BOUND('',#812,.T.);
#590=FACE_OUTER_BOUND('',#813,.T.);
#591=FACE_OUTER_BOUND('',#814,.T.);
#592=FACE_OUTER_BOUND('',#815,.T.);
#593=FACE_OUTER_BOUND('',#816,.T.);
#594=FACE_OUTER_BOUND('',#817,.T.);
#595=FACE_OUTER_BOUND('',#818,.T.);
#596=FACE_OUTER_BOUND('',#819,.T.);
#597=FACE_OUTER_BOUND('',#821,.T.);
#598=FACE_OUTER_BOUND('',#822,.T.);
#599=FACE_OUTER_BOUND('',#823,.T.);
#600=FACE_OUTER_BOUND('',#824,.T.);
#601=FACE_OUTER_BOUND('',#825,.T.);
#602=FACE_OUTER_BOUND('',#827,.T.);
#603=FACE_OUTER_BOUND('',#829,.T.);
#604=FACE_OUTER_BOUND('',#830,.T.);
#605=FACE_OUTER_BOUND('',#831,.T.);
#606=FACE_OUTER_BOUND('',#833,.T.);
#607=FACE_OUTER_BOUND('',#835,.T.);
#608=FACE_OUTER_BOUND('',#836,.T.);
#609=FACE_OUTER_BOUND('',#837,.T.);
#610=FACE_OUTER_BOUND('',#838,.T.);
#611=FACE_OUTER_BOUND('',#839,.T.);
#612=FACE_OUTER_BOUND('',#841,.T.);
#613=FACE_OUTER_BOUND('',#842,.T.);
#614=FACE_OUTER_BOUND('',#844,.T.);
#615=FACE_OUTER_BOUND('',#845,.T.);
#616=FACE_OUTER_BOUND('',#846,.T.);
#617=FACE_OUTER_BOUND('',#847,.T.);
#618=FACE_OUTER_BOUND('',#849,.T.);
#619=FACE_OUTER_BOUND('',#850,.T.);
#620=FACE_OUTER_BOUND('',#851,.T.);
#621=FACE_OUTER_BOUND('',#852,.T.);
#622=FACE_OUTER_BOUND('',#854,.T.);
#623=FACE_OUTER_BOUND('',#855,.T.);
#624=FACE_OUTER_BOUND('',#856,.T.);
#625=FACE_OUTER_BOUND('',#857,.T.);
#626=FACE_OUTER_BOUND('',#858,.T.);
#627=FACE_OUTER_BOUND('',#859,.T.);
#628=FACE_OUTER_BOUND('',#860,.T.);
#629=FACE_OUTER_BOUND('',#861,.T.);
#630=FACE_OUTER_BOUND('',#862,.T.);
#631=FACE_OUTER_BOUND('',#863,.T.);
#632=FACE_OUTER_BOUND('',#864,.T.);
#633=FACE_OUTER_BOUND('',#865,.T.);
#634=FACE_OUTER_BOUND('',#866,.T.);
#635=FACE_OUTER_BOUND('',#867,.T.);
#636=FACE_OUTER_BOUND('',#868,.T.);
#637=FACE_OUTER_BOUND('',#869,.T.);
#638=FACE_OUTER_BOUND('',#870,.T.);
#639=FACE_OUTER_BOUND('',#871,.T.);
#640=FACE_OUTER_BOUND('',#872,.T.);
#641=FACE_OUTER_BOUND('',#873,.T.);
#642=FACE_OUTER_BOUND('',#874,.T.);
#643=FACE_OUTER_BOUND('',#875,.T.);
#644=FACE_OUTER_BOUND('',#876,.T.);
#645=FACE_OUTER_BOUND('',#877,.T.);
#646=FACE_OUTER_BOUND('',#878,.T.);
#647=FACE_OUTER_BOUND('',#879,.T.);
#648=FACE_OUTER_BOUND('',#880,.T.);
#649=FACE_OUTER_BOUND('',#882,.T.);
#650=FACE_OUTER_BOUND('',#883,.T.);
#651=FACE_OUTER_BOUND('',#885,.T.);
#652=FACE_OUTER_BOUND('',#886,.T.);
#653=FACE_OUTER_BOUND('',#888,.T.);
#654=FACE_OUTER_BOUND('',#889,.T.);
#655=FACE_OUTER_BOUND('',#891,.T.);
#656=FACE_OUTER_BOUND('',#892,.T.);
#657=FACE_OUTER_BOUND('',#894,.T.);
#658=FACE_OUTER_BOUND('',#895,.T.);
#659=FACE_OUTER_BOUND('',#896,.T.);
#660=FACE_OUTER_BOUND('',#897,.T.);
#661=FACE_OUTER_BOUND('',#898,.T.);
#662=FACE_OUTER_BOUND('',#899,.T.);
#663=FACE_OUTER_BOUND('',#900,.T.);
#664=FACE_OUTER_BOUND('',#902,.T.);
#665=FACE_OUTER_BOUND('',#903,.T.);
#666=FACE_OUTER_BOUND('',#904,.T.);
#667=FACE_OUTER_BOUND('',#910,.T.);
#668=FACE_OUTER_BOUND('',#916,.T.);
#669=FACE_OUTER_BOUND('',#917,.T.);
#670=FACE_OUTER_BOUND('',#918,.T.);
#671=FACE_OUTER_BOUND('',#919,.T.);
#672=FACE_OUTER_BOUND('',#920,.T.);
#673=FACE_OUTER_BOUND('',#921,.T.);
#674=FACE_OUTER_BOUND('',#923,.T.);
#675=FACE_OUTER_BOUND('',#924,.T.);
#676=FACE_OUTER_BOUND('',#925,.T.);
#677=FACE_OUTER_BOUND('',#931,.T.);
#678=FACE_OUTER_BOUND('',#937,.T.);
#679=FACE_OUTER_BOUND('',#938,.T.);
#680=FACE_OUTER_BOUND('',#939,.T.);
#681=FACE_OUTER_BOUND('',#941,.T.);
#682=FACE_OUTER_BOUND('',#943,.T.);
#683=FACE_OUTER_BOUND('',#944,.T.);
#684=FACE_OUTER_BOUND('',#945,.T.);
#685=FACE_OUTER_BOUND('',#946,.T.);
#686=FACE_OUTER_BOUND('',#947,.T.);
#687=FACE_OUTER_BOUND('',#948,.T.);
#688=FACE_OUTER_BOUND('',#949,.T.);
#689=FACE_OUTER_BOUND('',#955,.T.);
#690=FACE_OUTER_BOUND('',#961,.T.);
#691=FACE_OUTER_BOUND('',#962,.T.);
#692=FACE_OUTER_BOUND('',#963,.T.);
#693=FACE_OUTER_BOUND('',#964,.T.);
#694=FACE_OUTER_BOUND('',#965,.T.);
#695=FACE_OUTER_BOUND('',#967,.T.);
#696=FACE_OUTER_BOUND('',#968,.T.);
#697=FACE_OUTER_BOUND('',#969,.T.);
#698=FACE_OUTER_BOUND('',#970,.T.);
#699=FACE_OUTER_BOUND('',#971,.T.);
#700=FACE_OUTER_BOUND('',#972,.T.);
#701=FACE_OUTER_BOUND('',#973,.T.);
#702=FACE_OUTER_BOUND('',#974,.T.);
#703=FACE_OUTER_BOUND('',#975,.T.);
#704=FACE_OUTER_BOUND('',#976,.T.);
#705=FACE_OUTER_BOUND('',#977,.T.);
#706=FACE_OUTER_BOUND('',#978,.T.);
#707=EDGE_LOOP('',(#2166,#2167,#2168,#2169));
#708=EDGE_LOOP('',(#2170,#2171,#2172,#2173));
#709=EDGE_LOOP('',(#2174,#2175,#2176,#2177));
#710=EDGE_LOOP('',(#2178,#2179,#2180,#2181));
#711=EDGE_LOOP('',(#2182));
#712=EDGE_LOOP('',(#2183));
#713=EDGE_LOOP('',(#2184,#2185,#2186,#2187));
#714=EDGE_LOOP('',(#2188,#2189,#2190,#2191));
#715=EDGE_LOOP('',(#2192,#2193,#2194,#2195));
#716=EDGE_LOOP('',(#2196,#2197,#2198,#2199));
#717=EDGE_LOOP('',(#2200,#2201,#2202,#2203));
#718=EDGE_LOOP('',(#2204,#2205,#2206,#2207));
#719=EDGE_LOOP('',(#2208));
#720=EDGE_LOOP('',(#2209,#2210,#2211,#2212));
#721=EDGE_LOOP('',(#2213,#2214,#2215,#2216));
#722=EDGE_LOOP('',(#2217));
#723=EDGE_LOOP('',(#2218,#2219,#2220,#2221));
#724=EDGE_LOOP('',(#2222,#2223,#2224,#2225));
#725=EDGE_LOOP('',(#2226,#2227,#2228,#2229));
#726=EDGE_LOOP('',(#2230));
#727=EDGE_LOOP('',(#2231));
#728=EDGE_LOOP('',(#2232,#2233,#2234,#2235));
#729=EDGE_LOOP('',(#2236,#2237,#2238,#2239));
#730=EDGE_LOOP('',(#2240,#2241,#2242,#2243));
#731=EDGE_LOOP('',(#2244,#2245,#2246,#2247));
#732=EDGE_LOOP('',(#2248));
#733=EDGE_LOOP('',(#2249));
#734=EDGE_LOOP('',(#2250,#2251,#2252,#2253));
#735=EDGE_LOOP('',(#2254,#2255,#2256,#2257));
#736=EDGE_LOOP('',(#2258,#2259,#2260,#2261));
#737=EDGE_LOOP('',(#2262,#2263,#2264,#2265));
#738=EDGE_LOOP('',(#2266,#2267,#2268,#2269));
#739=EDGE_LOOP('',(#2270,#2271,#2272,#2273));
#740=EDGE_LOOP('',(#2274));
#741=EDGE_LOOP('',(#2275,#2276,#2277,#2278));
#742=EDGE_LOOP('',(#2279,#2280,#2281,#2282));
#743=EDGE_LOOP('',(#2283));
#744=EDGE_LOOP('',(#2284,#2285,#2286,#2287));
#745=EDGE_LOOP('',(#2288,#2289,#2290,#2291));
#746=EDGE_LOOP('',(#2292,#2293,#2294,#2295));
#747=EDGE_LOOP('',(#2296));
#748=EDGE_LOOP('',(#2297));
#749=EDGE_LOOP('',(#2298,#2299,#2300,#2301));
#750=EDGE_LOOP('',(#2302));
#751=EDGE_LOOP('',(#2303,#2304,#2305,#2306));
#752=EDGE_LOOP('',(#2307));
#753=EDGE_LOOP('',(#2308));
#754=EDGE_LOOP('',(#2309));
#755=EDGE_LOOP('',(#2310));
#756=EDGE_LOOP('',(#2311));
#757=EDGE_LOOP('',(#2312,#2313,#2314,#2315));
#758=EDGE_LOOP('',(#2316,#2317,#2318,#2319));
#759=EDGE_LOOP('',(#2320,#2321,#2322,#2323));
#760=EDGE_LOOP('',(#2324));
#761=EDGE_LOOP('',(#2325));
#762=EDGE_LOOP('',(#2326));
#763=EDGE_LOOP('',(#2327));
#764=EDGE_LOOP('',(#2328,#2329,#2330,#2331));
#765=EDGE_LOOP('',(#2332,#2333,#2334,#2335));
#766=EDGE_LOOP('',(#2336));
#767=EDGE_LOOP('',(#2337));
#768=EDGE_LOOP('',(#2338));
#769=EDGE_LOOP('',(#2339));
#770=EDGE_LOOP('',(#2340,#2341,#2342,#2343));
#771=EDGE_LOOP('',(#2344,#2345,#2346,#2347));
#772=EDGE_LOOP('',(#2348));
#773=EDGE_LOOP('',(#2349));
#774=EDGE_LOOP('',(#2350));
#775=EDGE_LOOP('',(#2351));
#776=EDGE_LOOP('',(#2352,#2353,#2354,#2355));
#777=EDGE_LOOP('',(#2356,#2357,#2358,#2359));
#778=EDGE_LOOP('',(#2360,#2361,#2362,#2363));
#779=EDGE_LOOP('',(#2364,#2365,#2366,#2367));
#780=EDGE_LOOP('',(#2368,#2369,#2370,#2371));
#781=EDGE_LOOP('',(#2372,#2373,#2374,#2375));
#782=EDGE_LOOP('',(#2376,#2377,#2378,#2379));
#783=EDGE_LOOP('',(#2380,#2381,#2382,#2383));
#784=EDGE_LOOP('',(#2384,#2385,#2386,#2387));
#785=EDGE_LOOP('',(#2388));
#786=EDGE_LOOP('',(#2389));
#787=EDGE_LOOP('',(#2390));
#788=EDGE_LOOP('',(#2391));
#789=EDGE_LOOP('',(#2392,#2393,#2394,#2395));
#790=EDGE_LOOP('',(#2396));
#791=EDGE_LOOP('',(#2397));
#792=EDGE_LOOP('',(#2398));
#793=EDGE_LOOP('',(#2399));
#794=EDGE_LOOP('',(#2400,#2401,#2402,#2403));
#795=EDGE_LOOP('',(#2404,#2405,#2406,#2407));
#796=EDGE_LOOP('',(#2408,#2409,#2410,#2411));
#797=EDGE_LOOP('',(#2412,#2413,#2414,#2415));
#798=EDGE_LOOP('',(#2416,#2417,#2418,#2419));
#799=EDGE_LOOP('',(#2420,#2421,#2422,#2423));
#800=EDGE_LOOP('',(#2424,#2425,#2426,#2427));
#801=EDGE_LOOP('',(#2428,#2429,#2430,#2431));
#802=EDGE_LOOP('',(#2432));
#803=EDGE_LOOP('',(#2433));
#804=EDGE_LOOP('',(#2434));
#805=EDGE_LOOP('',(#2435));
#806=EDGE_LOOP('',(#2436,#2437,#2438,#2439));
#807=EDGE_LOOP('',(#2440,#2441,#2442,#2443));
#808=EDGE_LOOP('',(#2444,#2445,#2446,#2447));
#809=EDGE_LOOP('',(#2448,#2449,#2450,#2451));
#810=EDGE_LOOP('',(#2452,#2453,#2454,#2455));
#811=EDGE_LOOP('',(#2456,#2457,#2458,#2459));
#812=EDGE_LOOP('',(#2460,#2461,#2462,#2463,#2464,#2465));
#813=EDGE_LOOP('',(#2466,#2467,#2468,#2469,#2470,#2471));
#814=EDGE_LOOP('',(#2472));
#815=EDGE_LOOP('',(#2473));
#816=EDGE_LOOP('',(#2474,#2475,#2476,#2477));
#817=EDGE_LOOP('',(#2478,#2479,#2480,#2481));
#818=EDGE_LOOP('',(#2482,#2483,#2484,#2485));
#819=EDGE_LOOP('',(#2486));
#820=EDGE_LOOP('',(#2487));
#821=EDGE_LOOP('',(#2488,#2489,#2490,#2491));
#822=EDGE_LOOP('',(#2492,#2493,#2494,#2495));
#823=EDGE_LOOP('',(#2496,#2497,#2498,#2499));
#824=EDGE_LOOP('',(#2500,#2501,#2502,#2503));
#825=EDGE_LOOP('',(#2504));
#826=EDGE_LOOP('',(#2505));
#827=EDGE_LOOP('',(#2506));
#828=EDGE_LOOP('',(#2507));
#829=EDGE_LOOP('',(#2508,#2509,#2510,#2511));
#830=EDGE_LOOP('',(#2512,#2513,#2514,#2515));
#831=EDGE_LOOP('',(#2516));
#832=EDGE_LOOP('',(#2517));
#833=EDGE_LOOP('',(#2518));
#834=EDGE_LOOP('',(#2519));
#835=EDGE_LOOP('',(#2520,#2521,#2522,#2523,#2524,#2525));
#836=EDGE_LOOP('',(#2526,#2527,#2528,#2529,#2530));
#837=EDGE_LOOP('',(#2531,#2532,#2533,#2534));
#838=EDGE_LOOP('',(#2535,#2536,#2537,#2538));
#839=EDGE_LOOP('',(#2539));
#840=EDGE_LOOP('',(#2540));
#841=EDGE_LOOP('',(#2541,#2542,#2543,#2544,#2545));
#842=EDGE_LOOP('',(#2546));
#843=EDGE_LOOP('',(#2547));
#844=EDGE_LOOP('',(#2548,#2549,#2550,#2551));
#845=EDGE_LOOP('',(#2552,#2553,#2554,#2555,#2556,#2557));
#846=EDGE_LOOP('',(#2558,#2559,#2560,#2561,#2562));
#847=EDGE_LOOP('',(#2563));
#848=EDGE_LOOP('',(#2564));
#849=EDGE_LOOP('',(#2565,#2566,#2567,#2568));
#850=EDGE_LOOP('',(#2569,#2570,#2571,#2572));
#851=EDGE_LOOP('',(#2573,#2574,#2575,#2576));
#852=EDGE_LOOP('',(#2577));
#853=EDGE_LOOP('',(#2578));
#854=EDGE_LOOP('',(#2579,#2580,#2581,#2582,#2583));
#855=EDGE_LOOP('',(#2584,#2585));
#856=EDGE_LOOP('',(#2586,#2587));
#857=EDGE_LOOP('',(#2588,#2589));
#858=EDGE_LOOP('',(#2590,#2591));
#859=EDGE_LOOP('',(#2592,#2593));
#860=EDGE_LOOP('',(#2594,#2595));
#861=EDGE_LOOP('',(#2596,#2597));
#862=EDGE_LOOP('',(#2598,#2599));
#863=EDGE_LOOP('',(#2600,#2601,#2602,#2603));
#864=EDGE_LOOP('',(#2604,#2605,#2606,#2607,#2608,#2609,#2610,#2611,#2612,
#2613,#2614,#2615,#2616,#2617,#2618,#2619,#2620,#2621,#2622,#2623));
#865=EDGE_LOOP('',(#2624,#2625,#2626,#2627));
#866=EDGE_LOOP('',(#2628,#2629,#2630,#2631));
#867=EDGE_LOOP('',(#2632,#2633,#2634,#2635));
#868=EDGE_LOOP('',(#2636,#2637,#2638,#2639));
#869=EDGE_LOOP('',(#2640,#2641,#2642,#2643));
#870=EDGE_LOOP('',(#2644,#2645,#2646,#2647,#2648,#2649));
#871=EDGE_LOOP('',(#2650,#2651,#2652,#2653));
#872=EDGE_LOOP('',(#2654,#2655,#2656,#2657));
#873=EDGE_LOOP('',(#2658,#2659,#2660,#2661));
#874=EDGE_LOOP('',(#2662,#2663,#2664,#2665));
#875=EDGE_LOOP('',(#2666,#2667,#2668,#2669));
#876=EDGE_LOOP('',(#2670,#2671,#2672,#2673));
#877=EDGE_LOOP('',(#2674,#2675,#2676,#2677,#2678,#2679,#2680,#2681,#2682,
#2683,#2684,#2685,#2686,#2687,#2688,#2689,#2690,#2691,#2692,#2693));
#878=EDGE_LOOP('',(#2694,#2695,#2696,#2697));
#879=EDGE_LOOP('',(#2698,#2699,#2700,#2701));
#880=EDGE_LOOP('',(#2702));
#881=EDGE_LOOP('',(#2703));
#882=EDGE_LOOP('',(#2704,#2705,#2706,#2707));
#883=EDGE_LOOP('',(#2708));
#884=EDGE_LOOP('',(#2709));
#885=EDGE_LOOP('',(#2710,#2711,#2712,#2713));
#886=EDGE_LOOP('',(#2714));
#887=EDGE_LOOP('',(#2715));
#888=EDGE_LOOP('',(#2716,#2717,#2718,#2719));
#889=EDGE_LOOP('',(#2720));
#890=EDGE_LOOP('',(#2721));
#891=EDGE_LOOP('',(#2722,#2723,#2724,#2725));
#892=EDGE_LOOP('',(#2726));
#893=EDGE_LOOP('',(#2727));
#894=EDGE_LOOP('',(#2728,#2729,#2730,#2731));
#895=EDGE_LOOP('',(#2732,#2733,#2734,#2735));
#896=EDGE_LOOP('',(#2736,#2737,#2738,#2739));
#897=EDGE_LOOP('',(#2740,#2741,#2742,#2743));
#898=EDGE_LOOP('',(#2744,#2745,#2746,#2747));
#899=EDGE_LOOP('',(#2748,#2749,#2750,#2751));
#900=EDGE_LOOP('',(#2752));
#901=EDGE_LOOP('',(#2753));
#902=EDGE_LOOP('',(#2754,#2755,#2756,#2757));
#903=EDGE_LOOP('',(#2758,#2759,#2760,#2761));
#904=EDGE_LOOP('',(#2762));
#905=EDGE_LOOP('',(#2763));
#906=EDGE_LOOP('',(#2764));
#907=EDGE_LOOP('',(#2765));
#908=EDGE_LOOP('',(#2766));
#909=EDGE_LOOP('',(#2767));
#910=EDGE_LOOP('',(#2768));
#911=EDGE_LOOP('',(#2769));
#912=EDGE_LOOP('',(#2770));
#913=EDGE_LOOP('',(#2771));
#914=EDGE_LOOP('',(#2772));
#915=EDGE_LOOP('',(#2773));
#916=EDGE_LOOP('',(#2774,#2775,#2776,#2777));
#917=EDGE_LOOP('',(#2778,#2779,#2780,#2781));
#918=EDGE_LOOP('',(#2782,#2783,#2784,#2785));
#919=EDGE_LOOP('',(#2786,#2787,#2788,#2789));
#920=EDGE_LOOP('',(#2790,#2791,#2792,#2793));
#921=EDGE_LOOP('',(#2794));
#922=EDGE_LOOP('',(#2795));
#923=EDGE_LOOP('',(#2796,#2797,#2798,#2799));
#924=EDGE_LOOP('',(#2800,#2801,#2802,#2803));
#925=EDGE_LOOP('',(#2804));
#926=EDGE_LOOP('',(#2805));
#927=EDGE_LOOP('',(#2806));
#928=EDGE_LOOP('',(#2807));
#929=EDGE_LOOP('',(#2808));
#930=EDGE_LOOP('',(#2809));
#931=EDGE_LOOP('',(#2810));
#932=EDGE_LOOP('',(#2811));
#933=EDGE_LOOP('',(#2812));
#934=EDGE_LOOP('',(#2813));
#935=EDGE_LOOP('',(#2814));
#936=EDGE_LOOP('',(#2815));
#937=EDGE_LOOP('',(#2816,#2817,#2818,#2819));
#938=EDGE_LOOP('',(#2820,#2821,#2822,#2823));
#939=EDGE_LOOP('',(#2824));
#940=EDGE_LOOP('',(#2825));
#941=EDGE_LOOP('',(#2826));
#942=EDGE_LOOP('',(#2827));
#943=EDGE_LOOP('',(#2828,#2829,#2830,#2831));
#944=EDGE_LOOP('',(#2832,#2833,#2834,#2835));
#945=EDGE_LOOP('',(#2836,#2837,#2838,#2839));
#946=EDGE_LOOP('',(#2840,#2841,#2842,#2843));
#947=EDGE_LOOP('',(#2844,#2845,#2846,#2847));
#948=EDGE_LOOP('',(#2848,#2849,#2850,#2851));
#949=EDGE_LOOP('',(#2852));
#950=EDGE_LOOP('',(#2853));
#951=EDGE_LOOP('',(#2854));
#952=EDGE_LOOP('',(#2855));
#953=EDGE_LOOP('',(#2856));
#954=EDGE_LOOP('',(#2857));
#955=EDGE_LOOP('',(#2858));
#956=EDGE_LOOP('',(#2859));
#957=EDGE_LOOP('',(#2860));
#958=EDGE_LOOP('',(#2861));
#959=EDGE_LOOP('',(#2862));
#960=EDGE_LOOP('',(#2863));
#961=EDGE_LOOP('',(#2864));
#962=EDGE_LOOP('',(#2865,#2866,#2867,#2868));
#963=EDGE_LOOP('',(#2869,#2870,#2871,#2872));
#964=EDGE_LOOP('',(#2873,#2874,#2875,#2876));
#965=EDGE_LOOP('',(#2877));
#966=EDGE_LOOP('',(#2878));
#967=EDGE_LOOP('',(#2879,#2880,#2881,#2882));
#968=EDGE_LOOP('',(#2883,#2884,#2885,#2886));
#969=EDGE_LOOP('',(#2887,#2888,#2889,#2890));
#970=EDGE_LOOP('',(#2891));
#971=EDGE_LOOP('',(#2892,#2893,#2894,#2895));
#972=EDGE_LOOP('',(#2896,#2897,#2898,#2899));
#973=EDGE_LOOP('',(#2900,#2901,#2902,#2903));
#974=EDGE_LOOP('',(#2904,#2905,#2906,#2907));
#975=EDGE_LOOP('',(#2908,#2909,#2910,#2911));
#976=EDGE_LOOP('',(#2912,#2913,#2914,#2915));
#977=EDGE_LOOP('',(#2916,#2917,#2918,#2919,#2920,#2921));
#978=EDGE_LOOP('',(#2922,#2923,#2924,#2925,#2926,#2927));
#979=LINE('',#4957,#1161);
#980=LINE('',#4963,#1162);
#981=LINE('',#4969,#1163);
#982=LINE('',#4974,#1164);
#983=LINE('',#4976,#1165);
#984=LINE('',#4978,#1166);
#985=LINE('',#4979,#1167);
#986=LINE('',#4982,#1168);
#987=LINE('',#4984,#1169);
#988=LINE('',#4986,#1170);
#989=LINE('',#4987,#1171);
#990=LINE('',#4990,#1172);
#991=LINE('',#4992,#1173);
#992=LINE('',#4993,#1174);
#993=LINE('',#4996,#1175);
#994=LINE('',#4998,#1176);
#995=LINE('',#4999,#1177);
#996=LINE('',#5001,#1178);
#997=LINE('',#5003,#1179);
#998=LINE('',#5006,#1180);
#999=LINE('',#5008,#1181);
#1000=LINE('',#5009,#1182);
#1001=LINE('',#5012,#1183);
#1002=LINE('',#5013,#1184);
#1003=LINE('',#5016,#1185);
#1004=LINE('',#5017,#1186);
#1005=LINE('',#5019,#1187);
#1006=LINE('',#5027,#1188);
#1007=LINE('',#5033,#1189);
#1008=LINE('',#5039,#1190);
#1009=LINE('',#5044,#1191);
#1010=LINE('',#5046,#1192);
#1011=LINE('',#5048,#1193);
#1012=LINE('',#5049,#1194);
#1013=LINE('',#5052,#1195);
#1014=LINE('',#5054,#1196);
#1015=LINE('',#5056,#1197);
#1016=LINE('',#5057,#1198);
#1017=LINE('',#5060,#1199);
#1018=LINE('',#5062,#1200);
#1019=LINE('',#5063,#1201);
#1020=LINE('',#5066,#1202);
#1021=LINE('',#5068,#1203);
#1022=LINE('',#5069,#1204);
#1023=LINE('',#5071,#1205);
#1024=LINE('',#5073,#1206);
#1025=LINE('',#5076,#1207);
#1026=LINE('',#5078,#1208);
#1027=LINE('',#5079,#1209);
#1028=LINE('',#5082,#1210);
#1029=LINE('',#5083,#1211);
#1030=LINE('',#5086,#1212);
#1031=LINE('',#5087,#1213);
#1032=LINE('',#5089,#1214);
#1033=LINE('',#5097,#1215);
#1034=LINE('',#5104,#1216);
#1035=LINE('',#5118,#1217);
#1036=LINE('',#5121,#1218);
#1037=LINE('',#5126,#1219);
#1038=LINE('',#5134,#1220);
#1039=LINE('',#5140,#1221);
#1040=LINE('',#5149,#1222);
#1041=LINE('',#5155,#1223);
#1042=LINE('',#5164,#1224);
#1043=LINE('',#5170,#1225);
#1044=LINE('',#5176,#1226);
#1045=LINE('',#5182,#1227);
#1046=LINE('',#5187,#1228);
#1047=LINE('',#5189,#1229);
#1048=LINE('',#5191,#1230);
#1049=LINE('',#5192,#1231);
#1050=LINE('',#5195,#1232);
#1051=LINE('',#5197,#1233);
#1052=LINE('',#5198,#1234);
#1053=LINE('',#5201,#1235);
#1054=LINE('',#5203,#1236);
#1055=LINE('',#5204,#1237);
#1056=LINE('',#5206,#1238);
#1057=LINE('',#5207,#1239);
#1058=LINE('',#5214,#1240);
#1059=LINE('',#5216,#1241);
#1060=LINE('',#5218,#1242);
#1061=LINE('',#5219,#1243);
#1062=LINE('',#5222,#1244);
#1063=LINE('',#5224,#1245);
#1064=LINE('',#5225,#1246);
#1065=LINE('',#5228,#1247);
#1066=LINE('',#5230,#1248);
#1067=LINE('',#5231,#1249);
#1068=LINE('',#5233,#1250);
#1069=LINE('',#5234,#1251);
#1070=LINE('',#5242,#1252);
#1071=LINE('',#5248,#1253);
#1072=LINE('',#5256,#1254);
#1073=LINE('',#5258,#1255);
#1074=LINE('',#5260,#1256);
#1075=LINE('',#5261,#1257);
#1076=LINE('',#5264,#1258);
#1077=LINE('',#5266,#1259);
#1078=LINE('',#5267,#1260);
#1079=LINE('',#5270,#1261);
#1080=LINE('',#5272,#1262);
#1081=LINE('',#5273,#1263);
#1082=LINE('',#5276,#1264);
#1083=LINE('',#5278,#1265);
#1084=LINE('',#5279,#1266);
#1085=LINE('',#5282,#1267);
#1086=LINE('',#5284,#1268);
#1087=LINE('',#5285,#1269);
#1088=LINE('',#5287,#1270);
#1089=LINE('',#5288,#1271);
#1090=LINE('',#5300,#1272);
#1091=LINE('',#5304,#1273);
#1092=LINE('',#5308,#1274);
#1093=LINE('',#5315,#1275);
#1094=LINE('',#5317,#1276);
#1095=LINE('',#5323,#1277);
#1096=LINE('',#5329,#1278);
#1097=LINE('',#5338,#1279);
#1098=LINE('',#5344,#1280);
#1099=LINE('',#5362,#1281);
#1100=LINE('',#5368,#1282);
#1101=LINE('',#5372,#1283);
#1102=LINE('',#5378,#1284);
#1103=LINE('',#5383,#1285);
#1104=LINE('',#5398,#1286);
#1105=LINE('',#5407,#1287);
#1106=LINE('',#5411,#1288);
#1107=LINE('',#5415,#1289);
#1108=LINE('',#5418,#1290);
#1109=LINE('',#5571,#1291);
#1110=LINE('',#5867,#1292);
#1111=LINE('',#5909,#1293);
#1112=LINE('',#5914,#1294);
#1113=LINE('',#5923,#1295);
#1114=LINE('',#5928,#1296);
#1115=LINE('',#5940,#1297);
#1116=LINE('',#5946,#1298);
#1117=LINE('',#5952,#1299);
#1118=LINE('',#5958,#1300);
#1119=LINE('',#5964,#1301);
#1120=LINE('',#5971,#1302);
#1121=LINE('',#5977,#1303);
#1122=LINE('',#5986,#1304);
#1123=LINE('',#5992,#1305);
#1124=LINE('',#5998,#1306);
#1125=LINE('',#6004,#1307);
#1126=LINE('',#6010,#1308);
#1127=LINE('',#6018,#1309);
#1128=LINE('',#6023,#1310);
#1129=LINE('',#6032,#1311);
#1130=LINE('',#6038,#1312);
#1131=LINE('',#6047,#1313);
#1132=LINE('',#6053,#1314);
#1133=LINE('',#6059,#1315);
#1134=LINE('',#6065,#1316);
#1135=LINE('',#6071,#1317);
#1136=LINE('',#6077,#1318);
#1137=LINE('',#6088,#1319);
#1138=LINE('',#6092,#1320);
#1139=LINE('',#6096,#1321);
#1140=LINE('',#6103,#1322);
#1141=LINE('',#6107,#1323);
#1142=LINE('',#6111,#1324);
#1143=LINE('',#6116,#1325);
#1144=LINE('',#6118,#1326);
#1145=LINE('',#6120,#1327);
#1146=LINE('',#6121,#1328);
#1147=LINE('',#6124,#1329);
#1148=LINE('',#6126,#1330);
#1149=LINE('',#6127,#1331);
#1150=LINE('',#6130,#1332);
#1151=LINE('',#6132,#1333);
#1152=LINE('',#6133,#1334);
#1153=LINE('',#6136,#1335);
#1154=LINE('',#6138,#1336);
#1155=LINE('',#6139,#1337);
#1156=LINE('',#6142,#1338);
#1157=LINE('',#6144,#1339);
#1158=LINE('',#6145,#1340);
#1159=LINE('',#6147,#1341);
#1160=LINE('',#6148,#1342);
#1161=VECTOR('',#3896,0.33);
#1162=VECTOR('',#3903,0.33);
#1163=VECTOR('',#3910,0.505);
#1164=VECTOR('',#3915,1.);
#1165=VECTOR('',#3916,1.);
#1166=VECTOR('',#3917,1.);
#1167=VECTOR('',#3918,1.);
#1168=VECTOR('',#3919,1.);
#1169=VECTOR('',#3920,1.);
#1170=VECTOR('',#3921,1.);
#1171=VECTOR('',#3922,1.);
#1172=VECTOR('',#3925,1.);
#1173=VECTOR('',#3926,1.);
#1174=VECTOR('',#3927,1.);
#1175=VECTOR('',#3930,1.);
#1176=VECTOR('',#3931,1.);
#1177=VECTOR('',#3932,1.);
#1178=VECTOR('',#3935,1.);
#1179=VECTOR('',#3938,1.);
#1180=VECTOR('',#3941,1.);
#1181=VECTOR('',#3942,1.);
#1182=VECTOR('',#3943,1.);
#1183=VECTOR('',#3946,1.);
#1184=VECTOR('',#3947,1.);
#1185=VECTOR('',#3950,1.);
#1186=VECTOR('',#3951,1.);
#1187=VECTOR('',#3954,1.);
#1188=VECTOR('',#3965,0.33);
#1189=VECTOR('',#3972,0.33);
#1190=VECTOR('',#3979,0.505);
#1191=VECTOR('',#3984,1.);
#1192=VECTOR('',#3985,1.);
#1193=VECTOR('',#3986,1.);
#1194=VECTOR('',#3987,1.);
#1195=VECTOR('',#3988,1.);
#1196=VECTOR('',#3989,1.);
#1197=VECTOR('',#3990,1.);
#1198=VECTOR('',#3991,1.);
#1199=VECTOR('',#3994,1.);
#1200=VECTOR('',#3995,1.);
#1201=VECTOR('',#3996,1.);
#1202=VECTOR('',#3999,1.);
#1203=VECTOR('',#4000,1.);
#1204=VECTOR('',#4001,1.);
#1205=VECTOR('',#4004,1.);
#1206=VECTOR('',#4007,1.);
#1207=VECTOR('',#4010,1.);
#1208=VECTOR('',#4011,1.);
#1209=VECTOR('',#4012,1.);
#1210=VECTOR('',#4015,1.);
#1211=VECTOR('',#4016,1.);
#1212=VECTOR('',#4019,1.);
#1213=VECTOR('',#4020,1.);
#1214=VECTOR('',#4023,1.);
#1215=VECTOR('',#4034,0.165);
#1216=VECTOR('',#4043,0.165);
#1217=VECTOR('',#4062,0.6);
#1218=VECTOR('',#4065,0.5);
#1219=VECTOR('',#4072,0.5);
#1220=VECTOR('',#4083,0.505);
#1221=VECTOR('',#4090,0.8);
#1222=VECTOR('',#4103,0.505);
#1223=VECTOR('',#4110,0.8);
#1224=VECTOR('',#4123,0.25);
#1225=VECTOR('',#4130,0.25);
#1226=VECTOR('',#4137,0.25);
#1227=VECTOR('',#4144,0.25);
#1228=VECTOR('',#4149,1.);
#1229=VECTOR('',#4150,1.);
#1230=VECTOR('',#4151,1.);
#1231=VECTOR('',#4152,1.);
#1232=VECTOR('',#4155,1.);
#1233=VECTOR('',#4156,1.);
#1234=VECTOR('',#4157,1.);
#1235=VECTOR('',#4160,1.);
#1236=VECTOR('',#4161,1.);
#1237=VECTOR('',#4162,1.);
#1238=VECTOR('',#4165,1.);
#1239=VECTOR('',#4166,1.);
#1240=VECTOR('',#4175,1.);
#1241=VECTOR('',#4176,1.);
#1242=VECTOR('',#4177,1.);
#1243=VECTOR('',#4178,1.);
#1244=VECTOR('',#4181,1.);
#1245=VECTOR('',#4182,1.);
#1246=VECTOR('',#4183,1.);
#1247=VECTOR('',#4186,1.);
#1248=VECTOR('',#4187,1.);
#1249=VECTOR('',#4188,1.);
#1250=VECTOR('',#4191,1.);
#1251=VECTOR('',#4192,1.);
#1252=VECTOR('',#4203,0.32);
#1253=VECTOR('',#4210,0.6);
#1254=VECTOR('',#4221,1.);
#1255=VECTOR('',#4222,1.);
#1256=VECTOR('',#4223,1.);
#1257=VECTOR('',#4224,1.);
#1258=VECTOR('',#4227,1.);
#1259=VECTOR('',#4228,1.);
#1260=VECTOR('',#4229,1.);
#1261=VECTOR('',#4232,1.);
#1262=VECTOR('',#4233,1.);
#1263=VECTOR('',#4234,1.);
#1264=VECTOR('',#4237,1.);
#1265=VECTOR('',#4238,1.);
#1266=VECTOR('',#4239,1.);
#1267=VECTOR('',#4242,1.);
#1268=VECTOR('',#4243,1.);
#1269=VECTOR('',#4244,1.);
#1270=VECTOR('',#4247,1.);
#1271=VECTOR('',#4248,1.);
#1272=VECTOR('',#4265,0.475);
#1273=VECTOR('',#4270,0.5);
#1274=VECTOR('',#4275,0.485);
#1275=VECTOR('',#4284,0.31);
#1276=VECTOR('',#4287,0.3);
#1277=VECTOR('',#4294,0.225);
#1278=VECTOR('',#4301,1.1);
#1279=VECTOR('',#4314,0.605);
#1280=VECTOR('',#4321,1.);
#1281=VECTOR('',#4346,0.976185);
#1282=VECTOR('',#4353,0.5);
#1283=VECTOR('',#4358,0.53);
#1284=VECTOR('',#4367,0.976185);
#1285=VECTOR('',#4374,0.53);
#1286=VECTOR('',#4393,1.023815);
#1287=VECTOR('',#4404,1.47);
#1288=VECTOR('',#4409,1.5);
#1289=VECTOR('',#4414,1.47);
#1290=VECTOR('',#4419,1.023815);
#1291=VECTOR('',#4470,1.019052);
#1292=VECTOR('',#4547,0.980948);
#1293=VECTOR('',#4576,1.013815);
#1294=VECTOR('',#4583,0.991185);
#1295=VECTOR('',#4594,1.013815);
#1296=VECTOR('',#4601,0.991185);
#1297=VECTOR('',#4620,0.165);
#1298=VECTOR('',#4627,0.165);
#1299=VECTOR('',#4634,0.165);
#1300=VECTOR('',#4641,0.165);
#1301=VECTOR('',#4648,1.2);
#1302=VECTOR('',#4657,1.5);
#1303=VECTOR('',#4664,2.2);
#1304=VECTOR('',#4677,0.165);
#1305=VECTOR('',#4684,0.165);
#1306=VECTOR('',#4691,0.165);
#1307=VECTOR('',#4698,0.165);
#1308=VECTOR('',#4705,1.2);
#1309=VECTOR('',#4716,1.5);
#1310=VECTOR('',#4721,2.2);
#1311=VECTOR('',#4734,2.2);
#1312=VECTOR('',#4741,2.5);
#1313=VECTOR('',#4754,0.225);
#1314=VECTOR('',#4761,0.225);
#1315=VECTOR('',#4768,0.225);
#1316=VECTOR('',#4775,0.225);
#1317=VECTOR('',#4782,1.2);
#1318=VECTOR('',#4789,2.5);
#1319=VECTOR('',#4806,0.325);
#1320=VECTOR('',#4811,0.35);
#1321=VECTOR('',#4816,0.335);
#1322=VECTOR('',#4825,0.21);
#1323=VECTOR('',#4830,0.2);
#1324=VECTOR('',#4835,0.18);
#1325=VECTOR('',#4840,1.);
#1326=VECTOR('',#4841,1.);
#1327=VECTOR('',#4842,1.);
#1328=VECTOR('',#4843,1.);
#1329=VECTOR('',#4846,1.);
#1330=VECTOR('',#4847,1.);
#1331=VECTOR('',#4848,1.);
#1332=VECTOR('',#4851,1.);
#1333=VECTOR('',#4852,1.);
#1334=VECTOR('',#4853,1.);
#1335=VECTOR('',#4856,1.);
#1336=VECTOR('',#4857,1.);
#1337=VECTOR('',#4858,1.);
#1338=VECTOR('',#4861,1.);
#1339=VECTOR('',#4862,1.);
#1340=VECTOR('',#4863,1.);
#1341=VECTOR('',#4866,1.);
#1342=VECTOR('',#4867,1.);
#1343=CIRCLE('',#3449,0.33);
#1344=CIRCLE('',#3450,0.33);
#1345=CIRCLE('',#3452,0.33);
#1346=CIRCLE('',#3453,0.33);
#1347=CIRCLE('',#3455,0.505);
#1348=CIRCLE('',#3456,0.505);
#1349=CIRCLE('',#3470,0.33);
#1350=CIRCLE('',#3471,0.33);
#1351=CIRCLE('',#3473,0.33);
#1352=CIRCLE('',#3474,0.33);
#1353=CIRCLE('',#3476,0.505);
#1354=CIRCLE('',#3477,0.505);
#1355=CIRCLE('',#3491,0.165);
#1356=CIRCLE('',#3492,0.165);
#1357=CIRCLE('',#3495,0.165);
#1358=CIRCLE('',#3496,0.165);
#1359=CIRCLE('',#3499,0.6);
#1360=CIRCLE('',#3500,0.5);
#1361=CIRCLE('',#3502,0.6);
#1362=CIRCLE('',#3503,0.5);
#1363=CIRCLE('',#3506,0.5);
#1364=CIRCLE('',#3508,0.5);
#1365=CIRCLE('',#3513,0.505);
#1366=CIRCLE('',#3514,0.505);
#1367=CIRCLE('',#3516,0.8);
#1368=CIRCLE('',#3517,0.8);
#1369=CIRCLE('',#3522,0.505);
#1370=CIRCLE('',#3523,0.505);
#1371=CIRCLE('',#3525,0.8);
#1372=CIRCLE('',#3526,0.8);
#1373=CIRCLE('',#3531,0.25);
#1374=CIRCLE('',#3532,0.25);
#1375=CIRCLE('',#3534,0.25);
#1376=CIRCLE('',#3535,0.25);
#1377=CIRCLE('',#3537,0.25);
#1378=CIRCLE('',#3538,0.25);
#1379=CIRCLE('',#3540,0.25);
#1380=CIRCLE('',#3541,0.25);
#1381=CIRCLE('',#3557,0.32);
#1382=CIRCLE('',#3558,0.32);
#1383=CIRCLE('',#3560,0.6);
#1384=CIRCLE('',#3561,0.6);
#1385=CIRCLE('',#3574,0.2942);
#1386=CIRCLE('',#3576,0.45);
#1387=CIRCLE('',#3578,0.5);
#1388=CIRCLE('',#3580,0.5);
#1389=CIRCLE('',#3582,0.47);
#1390=CIRCLE('',#3584,0.32);
#1391=CIRCLE('',#3586,0.2942);
#1392=CIRCLE('',#3590,0.225);
#1393=CIRCLE('',#3591,0.225);
#1394=CIRCLE('',#3593,1.1);
#1395=CIRCLE('',#3594,1.1);
#1396=CIRCLE('',#3599,0.605);
#1397=CIRCLE('',#3600,0.605);
#1398=CIRCLE('',#3602,1.);
#1399=CIRCLE('',#3603,1.);
#1400=CIRCLE('',#3609,0.976185);
#1401=CIRCLE('',#3610,0.976185);
#1402=CIRCLE('',#3611,0.247676);
#1403=CIRCLE('',#3612,0.976185);
#1404=CIRCLE('',#3613,0.976185);
#1405=CIRCLE('',#3615,0.976185);
#1406=CIRCLE('',#3617,0.5);
#1407=CIRCLE('',#3618,0.5);
#1408=CIRCLE('',#3620,0.56);
#1409=CIRCLE('',#3623,0.976185);
#1410=CIRCLE('',#3625,0.56);
#1411=CIRCLE('',#3629,1.023815);
#1412=CIRCLE('',#3630,1.023815);
#1413=CIRCLE('',#3631,0.247676);
#1414=CIRCLE('',#3632,1.023815);
#1415=CIRCLE('',#3633,1.023815);
#1416=CIRCLE('',#3635,1.023815);
#1417=CIRCLE('',#3637,1.44);
#1418=CIRCLE('',#3638,1.023815);
#1419=CIRCLE('',#3640,1.5);
#1420=CIRCLE('',#3642,1.5);
#1421=CIRCLE('',#3644,1.44);
#1422=CIRCLE('',#3649,0.23815);
#1423=CIRCLE('',#3651,0.23815);
#1424=CIRCLE('',#3653,0.23815);
#1425=CIRCLE('',#3655,0.23815);
#1426=CIRCLE('',#3657,0.23815);
#1427=CIRCLE('',#3659,0.23815);
#1428=CIRCLE('',#3661,0.23815);
#1429=CIRCLE('',#3663,0.23815);
#1430=CIRCLE('',#3666,0.243053047864041);
#1431=CIRCLE('',#3667,0.243053047864041);
#1432=CIRCLE('',#3669,1.019052);
#1433=CIRCLE('',#3670,1.019052);
#1434=CIRCLE('',#3671,1.019052);
#1435=CIRCLE('',#3672,1.019052);
#1436=CIRCLE('',#3673,1.019052);
#1437=CIRCLE('',#3674,1.019052);
#1438=CIRCLE('',#3675,1.019052);
#1439=CIRCLE('',#3676,1.019052);
#1440=CIRCLE('',#3677,1.019052);
#1441=CIRCLE('',#3679,0.980948);
#1442=CIRCLE('',#3680,0.243053047864041);
#1443=CIRCLE('',#3682,0.243053047864041);
#1444=CIRCLE('',#3684,0.980948);
#1445=CIRCLE('',#3685,0.243053047864041);
#1446=CIRCLE('',#3687,0.243053047864041);
#1447=CIRCLE('',#3689,0.980948);
#1448=CIRCLE('',#3690,0.243053047864041);
#1449=CIRCLE('',#3692,0.243053047864041);
#1450=CIRCLE('',#3694,0.980948);
#1451=CIRCLE('',#3695,0.243053047864041);
#1452=CIRCLE('',#3697,0.243053047864041);
#1453=CIRCLE('',#3699,0.980948);
#1454=CIRCLE('',#3700,0.243053047864041);
#1455=CIRCLE('',#3702,0.243053047864041);
#1456=CIRCLE('',#3704,0.980948);
#1457=CIRCLE('',#3705,0.243053047864041);
#1458=CIRCLE('',#3707,0.243053047864041);
#1459=CIRCLE('',#3709,0.980948);
#1460=CIRCLE('',#3710,0.980948);
#1461=CIRCLE('',#3711,0.980948);
#1462=CIRCLE('',#3713,0.243053047864041);
#1463=CIRCLE('',#3715,0.243053047864041);
#1464=CIRCLE('',#3720,1.013815);
#1465=CIRCLE('',#3721,0.991185);
#1466=CIRCLE('',#3723,1.013815);
#1467=CIRCLE('',#3725,0.991185);
#1468=CIRCLE('',#3728,1.013815);
#1469=CIRCLE('',#3729,0.991185);
#1470=CIRCLE('',#3731,1.013815);
#1471=CIRCLE('',#3733,0.991185);
#1472=CIRCLE('',#3743,0.165);
#1473=CIRCLE('',#3744,0.165);
#1474=CIRCLE('',#3746,0.165);
#1475=CIRCLE('',#3747,0.165);
#1476=CIRCLE('',#3749,0.165);
#1477=CIRCLE('',#3750,0.165);
#1478=CIRCLE('',#3752,0.165);
#1479=CIRCLE('',#3753,0.165);
#1480=CIRCLE('',#3755,1.2);
#1481=CIRCLE('',#3756,1.2);
#1482=CIRCLE('',#3758,1.5);
#1483=CIRCLE('',#3760,1.5);
#1484=CIRCLE('',#3762,2.2);
#1485=CIRCLE('',#3763,2.2);
#1486=CIRCLE('',#3768,0.165);
#1487=CIRCLE('',#3769,0.165);
#1488=CIRCLE('',#3771,0.165);
#1489=CIRCLE('',#3772,0.165);
#1490=CIRCLE('',#3774,0.165);
#1491=CIRCLE('',#3775,0.165);
#1492=CIRCLE('',#3777,0.165);
#1493=CIRCLE('',#3778,0.165);
#1494=CIRCLE('',#3780,1.2);
#1495=CIRCLE('',#3781,1.2);
#1496=CIRCLE('',#3783,1.5);
#1497=CIRCLE('',#3785,1.5);
#1498=CIRCLE('',#3787,2.2);
#1499=CIRCLE('',#3788,2.2);
#1500=CIRCLE('',#3793,2.2);
#1501=CIRCLE('',#3794,2.2);
#1502=CIRCLE('',#3796,2.5);
#1503=CIRCLE('',#3797,2.5);
#1504=CIRCLE('',#3802,0.225);
#1505=CIRCLE('',#3803,0.225);
#1506=CIRCLE('',#3805,0.225);
#1507=CIRCLE('',#3806,0.225);
#1508=CIRCLE('',#3808,0.225);
#1509=CIRCLE('',#3809,0.225);
#1510=CIRCLE('',#3811,0.225);
#1511=CIRCLE('',#3812,0.225);
#1512=CIRCLE('',#3814,1.2);
#1513=CIRCLE('',#3815,1.2);
#1514=CIRCLE('',#3817,2.5);
#1515=CIRCLE('',#3818,2.5);
#1516=CIRCLE('',#3823,0.3);
#1517=CIRCLE('',#3825,0.35);
#1518=CIRCLE('',#3827,0.35);
#1519=CIRCLE('',#3829,0.32);
#1520=CIRCLE('',#3831,0.22);
#1521=CIRCLE('',#3833,0.1954);
#1522=CIRCLE('',#3835,0.1954);
#1523=CIRCLE('',#3837,0.16);
#1524=VERTEX_POINT('',#4954);
#1525=VERTEX_POINT('',#4956);
#1526=VERTEX_POINT('',#4960);
#1527=VERTEX_POINT('',#4962);
#1528=VERTEX_POINT('',#4966);
#1529=VERTEX_POINT('',#4968);
#1530=VERTEX_POINT('',#4972);
#1531=VERTEX_POINT('',#4973);
#1532=VERTEX_POINT('',#4975);
#1533=VERTEX_POINT('',#4977);
#1534=VERTEX_POINT('',#4980);
#1535=VERTEX_POINT('',#4981);
#1536=VERTEX_POINT('',#4983);
#1537=VERTEX_POINT('',#4985);
#1538=VERTEX_POINT('',#4989);
#1539=VERTEX_POINT('',#4991);
#1540=VERTEX_POINT('',#4995);
#1541=VERTEX_POINT('',#4997);
#1542=VERTEX_POINT('',#5005);
#1543=VERTEX_POINT('',#5007);
#1544=VERTEX_POINT('',#5011);
#1545=VERTEX_POINT('',#5015);
#1546=VERTEX_POINT('',#5024);
#1547=VERTEX_POINT('',#5026);
#1548=VERTEX_POINT('',#5030);
#1549=VERTEX_POINT('',#5032);
#1550=VERTEX_POINT('',#5036);
#1551=VERTEX_POINT('',#5038);
#1552=VERTEX_POINT('',#5042);
#1553=VERTEX_POINT('',#5043);
#1554=VERTEX_POINT('',#5045);
#1555=VERTEX_POINT('',#5047);
#1556=VERTEX_POINT('',#5050);
#1557=VERTEX_POINT('',#5051);
#1558=VERTEX_POINT('',#5053);
#1559=VERTEX_POINT('',#5055);
#1560=VERTEX_POINT('',#5059);
#1561=VERTEX_POINT('',#5061);
#1562=VERTEX_POINT('',#5065);
#1563=VERTEX_POINT('',#5067);
#1564=VERTEX_POINT('',#5075);
#1565=VERTEX_POINT('',#5077);
#1566=VERTEX_POINT('',#5081);
#1567=VERTEX_POINT('',#5085);
#1568=VERTEX_POINT('',#5094);
#1569=VERTEX_POINT('',#5096);
#1570=VERTEX_POINT('',#5101);
#1571=VERTEX_POINT('',#5103);
#1572=VERTEX_POINT('',#5108);
#1573=VERTEX_POINT('',#5110);
#1574=VERTEX_POINT('',#5113);
#1575=VERTEX_POINT('',#5115);
#1576=VERTEX_POINT('',#5120);
#1577=VERTEX_POINT('',#5124);
#1578=VERTEX_POINT('',#5131);
#1579=VERTEX_POINT('',#5133);
#1580=VERTEX_POINT('',#5137);
#1581=VERTEX_POINT('',#5139);
#1582=VERTEX_POINT('',#5146);
#1583=VERTEX_POINT('',#5148);
#1584=VERTEX_POINT('',#5152);
#1585=VERTEX_POINT('',#5154);
#1586=VERTEX_POINT('',#5161);
#1587=VERTEX_POINT('',#5163);
#1588=VERTEX_POINT('',#5167);
#1589=VERTEX_POINT('',#5169);
#1590=VERTEX_POINT('',#5173);
#1591=VERTEX_POINT('',#5175);
#1592=VERTEX_POINT('',#5179);
#1593=VERTEX_POINT('',#5181);
#1594=VERTEX_POINT('',#5185);
#1595=VERTEX_POINT('',#5186);
#1596=VERTEX_POINT('',#5188);
#1597=VERTEX_POINT('',#5190);
#1598=VERTEX_POINT('',#5194);
#1599=VERTEX_POINT('',#5196);
#1600=VERTEX_POINT('',#5200);
#1601=VERTEX_POINT('',#5202);
#1602=VERTEX_POINT('',#5212);
#1603=VERTEX_POINT('',#5213);
#1604=VERTEX_POINT('',#5215);
#1605=VERTEX_POINT('',#5217);
#1606=VERTEX_POINT('',#5221);
#1607=VERTEX_POINT('',#5223);
#1608=VERTEX_POINT('',#5227);
#1609=VERTEX_POINT('',#5229);
#1610=VERTEX_POINT('',#5239);
#1611=VERTEX_POINT('',#5241);
#1612=VERTEX_POINT('',#5245);
#1613=VERTEX_POINT('',#5247);
#1614=VERTEX_POINT('',#5254);
#1615=VERTEX_POINT('',#5255);
#1616=VERTEX_POINT('',#5257);
#1617=VERTEX_POINT('',#5259);
#1618=VERTEX_POINT('',#5263);
#1619=VERTEX_POINT('',#5265);
#1620=VERTEX_POINT('',#5269);
#1621=VERTEX_POINT('',#5271);
#1622=VERTEX_POINT('',#5275);
#1623=VERTEX_POINT('',#5277);
#1624=VERTEX_POINT('',#5281);
#1625=VERTEX_POINT('',#5283);
#1626=VERTEX_POINT('',#5292);
#1627=VERTEX_POINT('',#5295);
#1628=VERTEX_POINT('',#5298);
#1629=VERTEX_POINT('',#5302);
#1630=VERTEX_POINT('',#5306);
#1631=VERTEX_POINT('',#5310);
#1632=VERTEX_POINT('',#5313);
#1633=VERTEX_POINT('',#5320);
#1634=VERTEX_POINT('',#5322);
#1635=VERTEX_POINT('',#5326);
#1636=VERTEX_POINT('',#5328);
#1637=VERTEX_POINT('',#5335);
#1638=VERTEX_POINT('',#5337);
#1639=VERTEX_POINT('',#5341);
#1640=VERTEX_POINT('',#5343);
#1641=VERTEX_POINT('',#5351);
#1642=VERTEX_POINT('',#5352);
#1643=VERTEX_POINT('',#5355);
#1644=VERTEX_POINT('',#5357);
#1645=VERTEX_POINT('',#5361);
#1646=VERTEX_POINT('',#5365);
#1647=VERTEX_POINT('',#5367);
#1648=VERTEX_POINT('',#5371);
#1649=VERTEX_POINT('',#5376);
#1650=VERTEX_POINT('',#5380);
#1651=VERTEX_POINT('',#5386);
#1652=VERTEX_POINT('',#5387);
#1653=VERTEX_POINT('',#5390);
#1654=VERTEX_POINT('',#5392);
#1655=VERTEX_POINT('',#5396);
#1656=VERTEX_POINT('',#5400);
#1657=VERTEX_POINT('',#5402);
#1658=VERTEX_POINT('',#5405);
#1659=VERTEX_POINT('',#5409);
#1660=VERTEX_POINT('',#5413);
#1661=VERTEX_POINT('',#5421);
#1662=VERTEX_POINT('',#5422);
#1663=VERTEX_POINT('',#5425);
#1664=VERTEX_POINT('',#5426);
#1665=VERTEX_POINT('',#5429);
#1666=VERTEX_POINT('',#5430);
#1667=VERTEX_POINT('',#5433);
#1668=VERTEX_POINT('',#5434);
#1669=VERTEX_POINT('',#5437);
#1670=VERTEX_POINT('',#5438);
#1671=VERTEX_POINT('',#5441);
#1672=VERTEX_POINT('',#5442);
#1673=VERTEX_POINT('',#5445);
#1674=VERTEX_POINT('',#5446);
#1675=VERTEX_POINT('',#5449);
#1676=VERTEX_POINT('',#5450);
#1677=VERTEX_POINT('',#5454);
#1678=VERTEX_POINT('',#5455);
#1679=VERTEX_POINT('',#5478);
#1680=VERTEX_POINT('',#5480);
#1681=VERTEX_POINT('',#5505);
#1682=VERTEX_POINT('',#5507);
#1683=VERTEX_POINT('',#5530);
#1684=VERTEX_POINT('',#5532);
#1685=VERTEX_POINT('',#5555);
#1686=VERTEX_POINT('',#5557);
#1687=VERTEX_POINT('',#5570);
#1688=VERTEX_POINT('',#5573);
#1689=VERTEX_POINT('',#5586);
#1690=VERTEX_POINT('',#5588);
#1691=VERTEX_POINT('',#5611);
#1692=VERTEX_POINT('',#5613);
#1693=VERTEX_POINT('',#5636);
#1694=VERTEX_POINT('',#5638);
#1695=VERTEX_POINT('',#5661);
#1696=VERTEX_POINT('',#5663);
#1697=VERTEX_POINT('',#5688);
#1698=VERTEX_POINT('',#5692);
#1699=VERTEX_POINT('',#5717);
#1700=VERTEX_POINT('',#5721);
#1701=VERTEX_POINT('',#5746);
#1702=VERTEX_POINT('',#5750);
#1703=VERTEX_POINT('',#5751);
#1704=VERTEX_POINT('',#5778);
#1705=VERTEX_POINT('',#5782);
#1706=VERTEX_POINT('',#5807);
#1707=VERTEX_POINT('',#5811);
#1708=VERTEX_POINT('',#5836);
#1709=VERTEX_POINT('',#5840);
#1710=VERTEX_POINT('',#5865);
#1711=VERTEX_POINT('',#5868);
#1712=VERTEX_POINT('',#5870);
#1713=VERTEX_POINT('',#5902);
#1714=VERTEX_POINT('',#5904);
#1715=VERTEX_POINT('',#5907);
#1716=VERTEX_POINT('',#5911);
#1717=VERTEX_POINT('',#5916);
#1718=VERTEX_POINT('',#5918);
#1719=VERTEX_POINT('',#5921);
#1720=VERTEX_POINT('',#5925);
#1721=VERTEX_POINT('',#5937);
#1722=VERTEX_POINT('',#5939);
#1723=VERTEX_POINT('',#5943);
#1724=VERTEX_POINT('',#5945);
#1725=VERTEX_POINT('',#5949);
#1726=VERTEX_POINT('',#5951);
#1727=VERTEX_POINT('',#5955);
#1728=VERTEX_POINT('',#5957);
#1729=VERTEX_POINT('',#5961);
#1730=VERTEX_POINT('',#5963);
#1731=VERTEX_POINT('',#5967);
#1732=VERTEX_POINT('',#5970);
#1733=VERTEX_POINT('',#5974);
#1734=VERTEX_POINT('',#5976);
#1735=VERTEX_POINT('',#5983);
#1736=VERTEX_POINT('',#5985);
#1737=VERTEX_POINT('',#5989);
#1738=VERTEX_POINT('',#5991);
#1739=VERTEX_POINT('',#5995);
#1740=VERTEX_POINT('',#5997);
#1741=VERTEX_POINT('',#6001);
#1742=VERTEX_POINT('',#6003);
#1743=VERTEX_POINT('',#6007);
#1744=VERTEX_POINT('',#6009);
#1745=VERTEX_POINT('',#6013);
#1746=VERTEX_POINT('',#6016);
#1747=VERTEX_POINT('',#6020);
#1748=VERTEX_POINT('',#6022);
#1749=VERTEX_POINT('',#6029);
#1750=VERTEX_POINT('',#6031);
#1751=VERTEX_POINT('',#6035);
#1752=VERTEX_POINT('',#6037);
#1753=VERTEX_POINT('',#6044);
#1754=VERTEX_POINT('',#6046);
#1755=VERTEX_POINT('',#6050);
#1756=VERTEX_POINT('',#6052);
#1757=VERTEX_POINT('',#6056);
#1758=VERTEX_POINT('',#6058);
#1759=VERTEX_POINT('',#6062);
#1760=VERTEX_POINT('',#6064);
#1761=VERTEX_POINT('',#6068);
#1762=VERTEX_POINT('',#6070);
#1763=VERTEX_POINT('',#6074);
#1764=VERTEX_POINT('',#6076);
#1765=VERTEX_POINT('',#6083);
#1766=VERTEX_POINT('',#6086);
#1767=VERTEX_POINT('',#6090);
#1768=VERTEX_POINT('',#6094);
#1769=VERTEX_POINT('',#6098);
#1770=VERTEX_POINT('',#6101);
#1771=VERTEX_POINT('',#6105);
#1772=VERTEX_POINT('',#6109);
#1773=VERTEX_POINT('',#6114);
#1774=VERTEX_POINT('',#6115);
#1775=VERTEX_POINT('',#6117);
#1776=VERTEX_POINT('',#6119);
#1777=VERTEX_POINT('',#6123);
#1778=VERTEX_POINT('',#6125);
#1779=VERTEX_POINT('',#6129);
#1780=VERTEX_POINT('',#6131);
#1781=VERTEX_POINT('',#6135);
#1782=VERTEX_POINT('',#6137);
#1783=VERTEX_POINT('',#6141);
#1784=VERTEX_POINT('',#6143);
#1785=EDGE_CURVE('',#1524,#1524,#1343,.T.);
#1786=EDGE_CURVE('',#1524,#1525,#979,.T.);
#1787=EDGE_CURVE('',#1525,#1525,#1344,.T.);
#1788=EDGE_CURVE('',#1526,#1526,#1345,.T.);
#1789=EDGE_CURVE('',#1526,#1527,#980,.T.);
#1790=EDGE_CURVE('',#1527,#1527,#1346,.T.);
#1791=EDGE_CURVE('',#1528,#1528,#1347,.T.);
#1792=EDGE_CURVE('',#1528,#1529,#981,.T.);
#1793=EDGE_CURVE('',#1529,#1529,#1348,.T.);
#1794=EDGE_CURVE('',#1530,#1531,#982,.T.);
#1795=EDGE_CURVE('',#1530,#1532,#983,.T.);
#1796=EDGE_CURVE('',#1533,#1532,#984,.T.);
#1797=EDGE_CURVE('',#1531,#1533,#985,.T.);
#1798=EDGE_CURVE('',#1534,#1535,#986,.T.);
#1799=EDGE_CURVE('',#1536,#1534,#987,.T.);
#1800=EDGE_CURVE('',#1537,#1536,#988,.T.);
#1801=EDGE_CURVE('',#1535,#1537,#989,.T.);
#1802=EDGE_CURVE('',#1531,#1538,#990,.T.);
#1803=EDGE_CURVE('',#1539,#1533,#991,.T.);
#1804=EDGE_CURVE('',#1538,#1539,#992,.T.);
#1805=EDGE_CURVE('',#1540,#1530,#993,.T.);
#1806=EDGE_CURVE('',#1540,#1541,#994,.T.);
#1807=EDGE_CURVE('',#1532,#1541,#995,.T.);
#1808=EDGE_CURVE('',#1541,#1539,#996,.T.);
#1809=EDGE_CURVE('',#1538,#1540,#997,.T.);
#1810=EDGE_CURVE('',#1536,#1542,#998,.T.);
#1811=EDGE_CURVE('',#1543,#1542,#999,.T.);
#1812=EDGE_CURVE('',#1537,#1543,#1000,.T.);
#1813=EDGE_CURVE('',#1534,#1544,#1001,.T.);
#1814=EDGE_CURVE('',#1542,#1544,#1002,.T.);
#1815=EDGE_CURVE('',#1535,#1545,#1003,.T.);
#1816=EDGE_CURVE('',#1544,#1545,#1004,.T.);
#1817=EDGE_CURVE('',#1545,#1543,#1005,.T.);
#1818=EDGE_CURVE('',#1546,#1546,#1349,.T.);
#1819=EDGE_CURVE('',#1546,#1547,#1006,.T.);
#1820=EDGE_CURVE('',#1547,#1547,#1350,.T.);
#1821=EDGE_CURVE('',#1548,#1548,#1351,.T.);
#1822=EDGE_CURVE('',#1548,#1549,#1007,.T.);
#1823=EDGE_CURVE('',#1549,#1549,#1352,.T.);
#1824=EDGE_CURVE('',#1550,#1550,#1353,.T.);
#1825=EDGE_CURVE('',#1550,#1551,#1008,.T.);
#1826=EDGE_CURVE('',#1551,#1551,#1354,.T.);
#1827=EDGE_CURVE('',#1552,#1553,#1009,.T.);
#1828=EDGE_CURVE('',#1552,#1554,#1010,.T.);
#1829=EDGE_CURVE('',#1555,#1554,#1011,.T.);
#1830=EDGE_CURVE('',#1553,#1555,#1012,.T.);
#1831=EDGE_CURVE('',#1556,#1557,#1013,.T.);
#1832=EDGE_CURVE('',#1558,#1556,#1014,.T.);
#1833=EDGE_CURVE('',#1559,#1558,#1015,.T.);
#1834=EDGE_CURVE('',#1557,#1559,#1016,.T.);
#1835=EDGE_CURVE('',#1553,#1560,#1017,.T.);
#1836=EDGE_CURVE('',#1561,#1555,#1018,.T.);
#1837=EDGE_CURVE('',#1560,#1561,#1019,.T.);
#1838=EDGE_CURVE('',#1562,#1552,#1020,.T.);
#1839=EDGE_CURVE('',#1562,#1563,#1021,.T.);
#1840=EDGE_CURVE('',#1554,#1563,#1022,.T.);
#1841=EDGE_CURVE('',#1563,#1561,#1023,.T.);
#1842=EDGE_CURVE('',#1560,#1562,#1024,.T.);
#1843=EDGE_CURVE('',#1558,#1564,#1025,.T.);
#1844=EDGE_CURVE('',#1565,#1564,#1026,.T.);
#1845=EDGE_CURVE('',#1559,#1565,#1027,.T.);
#1846=EDGE_CURVE('',#1556,#1566,#1028,.T.);
#1847=EDGE_CURVE('',#1564,#1566,#1029,.T.);
#1848=EDGE_CURVE('',#1557,#1567,#1030,.T.);
#1849=EDGE_CURVE('',#1566,#1567,#1031,.T.);
#1850=EDGE_CURVE('',#1567,#1565,#1032,.T.);
#1851=EDGE_CURVE('',#1568,#1568,#1355,.T.);
#1852=EDGE_CURVE('',#1568,#1569,#1033,.T.);
#1853=EDGE_CURVE('',#1569,#1569,#1356,.T.);
#1854=EDGE_CURVE('',#1570,#1570,#1357,.T.);
#1855=EDGE_CURVE('',#1570,#1571,#1034,.T.);
#1856=EDGE_CURVE('',#1571,#1571,#1358,.T.);
#1857=EDGE_CURVE('',#1572,#1572,#1359,.T.);
#1858=EDGE_CURVE('',#1573,#1573,#1360,.T.);
#1859=EDGE_CURVE('',#1574,#1574,#1361,.T.);
#1860=EDGE_CURVE('',#1575,#1575,#1362,.T.);
#1861=EDGE_CURVE('',#1572,#1574,#1035,.T.);
#1862=EDGE_CURVE('',#1575,#1576,#1036,.T.);
#1863=EDGE_CURVE('',#1576,#1576,#1363,.T.);
#1864=EDGE_CURVE('',#1577,#1577,#1364,.T.);
#1865=EDGE_CURVE('',#1577,#1573,#1037,.T.);
#1866=EDGE_CURVE('',#1578,#1578,#1365,.T.);
#1867=EDGE_CURVE('',#1578,#1579,#1038,.T.);
#1868=EDGE_CURVE('',#1579,#1579,#1366,.T.);
#1869=EDGE_CURVE('',#1580,#1580,#1367,.T.);
#1870=EDGE_CURVE('',#1580,#1581,#1039,.T.);
#1871=EDGE_CURVE('',#1581,#1581,#1368,.T.);
#1872=EDGE_CURVE('',#1582,#1582,#1369,.T.);
#1873=EDGE_CURVE('',#1582,#1583,#1040,.T.);
#1874=EDGE_CURVE('',#1583,#1583,#1370,.T.);
#1875=EDGE_CURVE('',#1584,#1584,#1371,.T.);
#1876=EDGE_CURVE('',#1584,#1585,#1041,.T.);
#1877=EDGE_CURVE('',#1585,#1585,#1372,.T.);
#1878=EDGE_CURVE('',#1586,#1586,#1373,.T.);
#1879=EDGE_CURVE('',#1586,#1587,#1042,.T.);
#1880=EDGE_CURVE('',#1587,#1587,#1374,.T.);
#1881=EDGE_CURVE('',#1588,#1588,#1375,.T.);
#1882=EDGE_CURVE('',#1588,#1589,#1043,.T.);
#1883=EDGE_CURVE('',#1589,#1589,#1376,.T.);
#1884=EDGE_CURVE('',#1590,#1590,#1377,.T.);
#1885=EDGE_CURVE('',#1590,#1591,#1044,.T.);
#1886=EDGE_CURVE('',#1591,#1591,#1378,.T.);
#1887=EDGE_CURVE('',#1592,#1592,#1379,.T.);
#1888=EDGE_CURVE('',#1592,#1593,#1045,.T.);
#1889=EDGE_CURVE('',#1593,#1593,#1380,.T.);
#1890=EDGE_CURVE('',#1594,#1595,#1046,.T.);
#1891=EDGE_CURVE('',#1595,#1596,#1047,.T.);
#1892=EDGE_CURVE('',#1597,#1596,#1048,.T.);
#1893=EDGE_CURVE('',#1594,#1597,#1049,.T.);
#1894=EDGE_CURVE('',#1598,#1594,#1050,.T.);
#1895=EDGE_CURVE('',#1599,#1597,#1051,.T.);
#1896=EDGE_CURVE('',#1598,#1599,#1052,.T.);
#1897=EDGE_CURVE('',#1600,#1598,#1053,.T.);
#1898=EDGE_CURVE('',#1601,#1599,#1054,.T.);
#1899=EDGE_CURVE('',#1600,#1601,#1055,.T.);
#1900=EDGE_CURVE('',#1595,#1600,#1056,.T.);
#1901=EDGE_CURVE('',#1596,#1601,#1057,.T.);
#1902=EDGE_CURVE('',#1602,#1603,#1058,.T.);
#1903=EDGE_CURVE('',#1603,#1604,#1059,.T.);
#1904=EDGE_CURVE('',#1605,#1604,#1060,.T.);
#1905=EDGE_CURVE('',#1602,#1605,#1061,.T.);
#1906=EDGE_CURVE('',#1606,#1602,#1062,.T.);
#1907=EDGE_CURVE('',#1607,#1605,#1063,.T.);
#1908=EDGE_CURVE('',#1606,#1607,#1064,.T.);
#1909=EDGE_CURVE('',#1608,#1606,#1065,.T.);
#1910=EDGE_CURVE('',#1609,#1607,#1066,.T.);
#1911=EDGE_CURVE('',#1608,#1609,#1067,.T.);
#1912=EDGE_CURVE('',#1603,#1608,#1068,.T.);
#1913=EDGE_CURVE('',#1604,#1609,#1069,.T.);
#1914=EDGE_CURVE('',#1610,#1610,#1381,.T.);
#1915=EDGE_CURVE('',#1610,#1611,#1070,.T.);
#1916=EDGE_CURVE('',#1611,#1611,#1382,.T.);
#1917=EDGE_CURVE('',#1612,#1612,#1383,.T.);
#1918=EDGE_CURVE('',#1612,#1613,#1071,.T.);
#1919=EDGE_CURVE('',#1613,#1613,#1384,.T.);
#1920=EDGE_CURVE('',#1614,#1615,#1072,.T.);
#1921=EDGE_CURVE('',#1615,#1616,#1073,.T.);
#1922=EDGE_CURVE('',#1616,#1617,#1074,.T.);
#1923=EDGE_CURVE('',#1614,#1617,#1075,.T.);
#1924=EDGE_CURVE('',#1615,#1618,#1076,.T.);
#1925=EDGE_CURVE('',#1618,#1619,#1077,.T.);
#1926=EDGE_CURVE('',#1619,#1616,#1078,.T.);
#1927=EDGE_CURVE('',#1618,#1620,#1079,.T.);
#1928=EDGE_CURVE('',#1620,#1621,#1080,.T.);
#1929=EDGE_CURVE('',#1621,#1619,#1081,.T.);
#1930=EDGE_CURVE('',#1620,#1622,#1082,.T.);
#1931=EDGE_CURVE('',#1622,#1623,#1083,.T.);
#1932=EDGE_CURVE('',#1623,#1621,#1084,.T.);
#1933=EDGE_CURVE('',#1622,#1624,#1085,.T.);
#1934=EDGE_CURVE('',#1624,#1625,#1086,.T.);
#1935=EDGE_CURVE('',#1625,#1623,#1087,.T.);
#1936=EDGE_CURVE('',#1624,#1614,#1088,.T.);
#1937=EDGE_CURVE('',#1617,#1625,#1089,.T.);
#1938=EDGE_CURVE('',#1626,#1626,#1385,.T.);
#1939=EDGE_CURVE('',#1627,#1627,#1386,.T.);
#1940=EDGE_CURVE('',#1628,#1628,#1387,.T.);
#1941=EDGE_CURVE('',#1628,#1627,#1090,.T.);
#1942=EDGE_CURVE('',#1629,#1629,#1388,.T.);
#1943=EDGE_CURVE('',#1629,#1628,#1091,.T.);
#1944=EDGE_CURVE('',#1630,#1630,#1389,.T.);
#1945=EDGE_CURVE('',#1630,#1629,#1092,.T.);
#1946=EDGE_CURVE('',#1631,#1631,#1390,.T.);
#1947=EDGE_CURVE('',#1632,#1632,#1391,.F.);
#1948=EDGE_CURVE('',#1632,#1631,#1093,.T.);
#1949=EDGE_CURVE('',#1626,#1632,#1094,.T.);
#1950=EDGE_CURVE('',#1633,#1633,#1392,.T.);
#1951=EDGE_CURVE('',#1633,#1634,#1095,.T.);
#1952=EDGE_CURVE('',#1634,#1634,#1393,.T.);
#1953=EDGE_CURVE('',#1635,#1635,#1394,.T.);
#1954=EDGE_CURVE('',#1635,#1636,#1096,.T.);
#1955=EDGE_CURVE('',#1636,#1636,#1395,.T.);
#1956=EDGE_CURVE('',#1637,#1637,#1396,.T.);
#1957=EDGE_CURVE('',#1637,#1638,#1097,.T.);
#1958=EDGE_CURVE('',#1638,#1638,#1397,.T.);
#1959=EDGE_CURVE('',#1639,#1639,#1398,.T.);
#1960=EDGE_CURVE('',#1639,#1640,#1098,.T.);
#1961=EDGE_CURVE('',#1640,#1640,#1399,.T.);
#1962=EDGE_CURVE('',#1641,#1642,#1400,.T.);
#1963=EDGE_CURVE('',#1642,#1641,#1401,.T.);
#1964=EDGE_CURVE('',#1642,#1643,#1402,.T.);
#1965=EDGE_CURVE('',#1644,#1643,#1403,.T.);
#1966=EDGE_CURVE('',#1643,#1644,#1404,.T.);
#1967=EDGE_CURVE('',#1644,#1645,#1099,.T.);
#1968=EDGE_CURVE('',#1645,#1645,#1405,.T.);
#1969=EDGE_CURVE('',#1646,#1646,#1406,.T.);
#1970=EDGE_CURVE('',#1646,#1647,#1100,.T.);
#1971=EDGE_CURVE('',#1647,#1647,#1407,.T.);
#1972=EDGE_CURVE('',#1647,#1648,#1101,.T.);
#1973=EDGE_CURVE('',#1648,#1648,#1408,.T.);
#1974=EDGE_CURVE('',#1649,#1649,#1409,.T.);
#1975=EDGE_CURVE('',#1649,#1641,#1102,.T.);
#1976=EDGE_CURVE('',#1650,#1650,#1410,.T.);
#1977=EDGE_CURVE('',#1650,#1646,#1103,.T.);
#1978=EDGE_CURVE('',#1651,#1652,#1411,.T.);
#1979=EDGE_CURVE('',#1652,#1651,#1412,.T.);
#1980=EDGE_CURVE('',#1652,#1653,#1413,.T.);
#1981=EDGE_CURVE('',#1654,#1653,#1414,.T.);
#1982=EDGE_CURVE('',#1653,#1654,#1415,.T.);
#1983=EDGE_CURVE('',#1655,#1655,#1416,.T.);
#1984=EDGE_CURVE('',#1655,#1654,#1104,.T.);
#1985=EDGE_CURVE('',#1656,#1656,#1417,.T.);
#1986=EDGE_CURVE('',#1657,#1657,#1418,.T.);
#1987=EDGE_CURVE('',#1658,#1658,#1419,.T.);
#1988=EDGE_CURVE('',#1658,#1656,#1105,.T.);
#1989=EDGE_CURVE('',#1659,#1659,#1420,.T.);
#1990=EDGE_CURVE('',#1659,#1658,#1106,.T.);
#1991=EDGE_CURVE('',#1660,#1660,#1421,.T.);
#1992=EDGE_CURVE('',#1660,#1659,#1107,.T.);
#1993=EDGE_CURVE('',#1651,#1657,#1108,.T.);
#1994=EDGE_CURVE('',#1661,#1662,#1422,.T.);
#1995=EDGE_CURVE('',#1663,#1664,#1423,.T.);
#1996=EDGE_CURVE('',#1665,#1666,#1424,.T.);
#1997=EDGE_CURVE('',#1667,#1668,#1425,.T.);
#1998=EDGE_CURVE('',#1669,#1670,#1426,.T.);
#1999=EDGE_CURVE('',#1671,#1672,#1427,.T.);
#2000=EDGE_CURVE('',#1673,#1674,#1428,.T.);
#2001=EDGE_CURVE('',#1675,#1676,#1429,.T.);
#2002=EDGE_CURVE('',#1677,#1678,#187,.T.);
#2003=EDGE_CURVE('',#1679,#1677,#1430,.T.);
#2004=EDGE_CURVE('',#1680,#1679,#188,.T.);
#2005=EDGE_CURVE('',#1678,#1680,#1431,.T.);
#2006=EDGE_CURVE('',#1681,#1679,#1432,.T.);
#2007=EDGE_CURVE('',#1681,#1682,#189,.T.);
#2008=EDGE_CURVE('',#1683,#1682,#1433,.T.);
#2009=EDGE_CURVE('',#1683,#1684,#190,.T.);
#2010=EDGE_CURVE('',#1685,#1684,#1434,.T.);
#2011=EDGE_CURVE('',#1685,#1686,#191,.T.);
#2012=EDGE_CURVE('',#1686,#1687,#1109,.T.);
#2013=EDGE_CURVE('',#1687,#1687,#1435,.T.);
#2014=EDGE_CURVE('',#1686,#1688,#192,.T.);
#2015=EDGE_CURVE('',#1689,#1688,#1436,.T.);
#2016=EDGE_CURVE('',#1689,#1690,#193,.T.);
#2017=EDGE_CURVE('',#1691,#1690,#1437,.T.);
#2018=EDGE_CURVE('',#1691,#1692,#194,.T.);
#2019=EDGE_CURVE('',#1693,#1692,#1438,.T.);
#2020=EDGE_CURVE('',#1693,#1694,#195,.T.);
#2021=EDGE_CURVE('',#1695,#1694,#1439,.T.);
#2022=EDGE_CURVE('',#1695,#1696,#196,.T.);
#2023=EDGE_CURVE('',#1680,#1696,#1440,.T.);
#2024=EDGE_CURVE('',#1677,#1697,#1441,.T.);
#2025=EDGE_CURVE('',#1697,#1681,#1442,.T.);
#2026=EDGE_CURVE('',#1698,#1697,#197,.T.);
#2027=EDGE_CURVE('',#1682,#1698,#1443,.T.);
#2028=EDGE_CURVE('',#1698,#1699,#1444,.T.);
#2029=EDGE_CURVE('',#1699,#1683,#1445,.T.);
#2030=EDGE_CURVE('',#1700,#1699,#198,.T.);
#2031=EDGE_CURVE('',#1684,#1700,#1446,.T.);
#2032=EDGE_CURVE('',#1700,#1701,#1447,.T.);
#2033=EDGE_CURVE('',#1701,#1685,#1448,.T.);
#2034=EDGE_CURVE('',#1702,#1703,#199,.T.);
#2035=EDGE_CURVE('',#1688,#1702,#1449,.T.);
#2036=EDGE_CURVE('',#1703,#1701,#200,.T.);
#2037=EDGE_CURVE('',#1702,#1704,#1450,.T.);
#2038=EDGE_CURVE('',#1704,#1689,#1451,.T.);
#2039=EDGE_CURVE('',#1705,#1704,#201,.T.);
#2040=EDGE_CURVE('',#1690,#1705,#1452,.T.);
#2041=EDGE_CURVE('',#1705,#1706,#1453,.T.);
#2042=EDGE_CURVE('',#1706,#1691,#1454,.T.);
#2043=EDGE_CURVE('',#1707,#1706,#202,.T.);
#2044=EDGE_CURVE('',#1692,#1707,#1455,.T.);
#2045=EDGE_CURVE('',#1707,#1708,#1456,.T.);
#2046=EDGE_CURVE('',#1708,#1693,#1457,.T.);
#2047=EDGE_CURVE('',#1709,#1708,#203,.T.);
#2048=EDGE_CURVE('',#1694,#1709,#1458,.T.);
#2049=EDGE_CURVE('',#1710,#1710,#1459,.T.);
#2050=EDGE_CURVE('',#1710,#1703,#1110,.T.);
#2051=EDGE_CURVE('',#1711,#1678,#1460,.T.);
#2052=EDGE_CURVE('',#1711,#1712,#204,.T.);
#2053=EDGE_CURVE('',#1709,#1712,#1461,.T.);
#2054=EDGE_CURVE('',#1696,#1711,#1462,.T.);
#2055=EDGE_CURVE('',#1712,#1695,#1463,.T.);
#2056=EDGE_CURVE('',#1713,#1713,#1464,.T.);
#2057=EDGE_CURVE('',#1714,#1714,#1465,.T.);
#2058=EDGE_CURVE('',#1715,#1715,#1466,.T.);
#2059=EDGE_CURVE('',#1715,#1713,#1111,.T.);
#2060=EDGE_CURVE('',#1716,#1716,#1467,.T.);
#2061=EDGE_CURVE('',#1716,#1714,#1112,.T.);
#2062=EDGE_CURVE('',#1717,#1717,#1468,.T.);
#2063=EDGE_CURVE('',#1718,#1718,#1469,.T.);
#2064=EDGE_CURVE('',#1719,#1719,#1470,.T.);
#2065=EDGE_CURVE('',#1719,#1717,#1113,.T.);
#2066=EDGE_CURVE('',#1720,#1720,#1471,.T.);
#2067=EDGE_CURVE('',#1720,#1718,#1114,.T.);
#2068=EDGE_CURVE('',#1721,#1721,#1472,.T.);
#2069=EDGE_CURVE('',#1721,#1722,#1115,.T.);
#2070=EDGE_CURVE('',#1722,#1722,#1473,.T.);
#2071=EDGE_CURVE('',#1723,#1723,#1474,.T.);
#2072=EDGE_CURVE('',#1723,#1724,#1116,.T.);
#2073=EDGE_CURVE('',#1724,#1724,#1475,.T.);
#2074=EDGE_CURVE('',#1725,#1725,#1476,.T.);
#2075=EDGE_CURVE('',#1725,#1726,#1117,.T.);
#2076=EDGE_CURVE('',#1726,#1726,#1477,.T.);
#2077=EDGE_CURVE('',#1727,#1727,#1478,.T.);
#2078=EDGE_CURVE('',#1727,#1728,#1118,.T.);
#2079=EDGE_CURVE('',#1728,#1728,#1479,.T.);
#2080=EDGE_CURVE('',#1729,#1729,#1480,.T.);
#2081=EDGE_CURVE('',#1729,#1730,#1119,.T.);
#2082=EDGE_CURVE('',#1730,#1730,#1481,.T.);
#2083=EDGE_CURVE('',#1731,#1731,#1482,.T.);
#2084=EDGE_CURVE('',#1731,#1732,#1120,.T.);
#2085=EDGE_CURVE('',#1732,#1732,#1483,.T.);
#2086=EDGE_CURVE('',#1733,#1733,#1484,.T.);
#2087=EDGE_CURVE('',#1733,#1734,#1121,.T.);
#2088=EDGE_CURVE('',#1734,#1734,#1485,.T.);
#2089=EDGE_CURVE('',#1735,#1735,#1486,.T.);
#2090=EDGE_CURVE('',#1735,#1736,#1122,.T.);
#2091=EDGE_CURVE('',#1736,#1736,#1487,.T.);
#2092=EDGE_CURVE('',#1737,#1737,#1488,.T.);
#2093=EDGE_CURVE('',#1737,#1738,#1123,.T.);
#2094=EDGE_CURVE('',#1738,#1738,#1489,.T.);
#2095=EDGE_CURVE('',#1739,#1739,#1490,.T.);
#2096=EDGE_CURVE('',#1739,#1740,#1124,.T.);
#2097=EDGE_CURVE('',#1740,#1740,#1491,.T.);
#2098=EDGE_CURVE('',#1741,#1741,#1492,.T.);
#2099=EDGE_CURVE('',#1741,#1742,#1125,.T.);
#2100=EDGE_CURVE('',#1742,#1742,#1493,.T.);
#2101=EDGE_CURVE('',#1743,#1743,#1494,.T.);
#2102=EDGE_CURVE('',#1743,#1744,#1126,.T.);
#2103=EDGE_CURVE('',#1744,#1744,#1495,.T.);
#2104=EDGE_CURVE('',#1745,#1745,#1496,.T.);
#2105=EDGE_CURVE('',#1746,#1746,#1497,.T.);
#2106=EDGE_CURVE('',#1746,#1745,#1127,.T.);
#2107=EDGE_CURVE('',#1747,#1747,#1498,.T.);
#2108=EDGE_CURVE('',#1747,#1748,#1128,.T.);
#2109=EDGE_CURVE('',#1748,#1748,#1499,.T.);
#2110=EDGE_CURVE('',#1749,#1749,#1500,.T.);
#2111=EDGE_CURVE('',#1749,#1750,#1129,.T.);
#2112=EDGE_CURVE('',#1750,#1750,#1501,.T.);
#2113=EDGE_CURVE('',#1751,#1751,#1502,.T.);
#2114=EDGE_CURVE('',#1751,#1752,#1130,.T.);
#2115=EDGE_CURVE('',#1752,#1752,#1503,.T.);
#2116=EDGE_CURVE('',#1753,#1753,#1504,.T.);
#2117=EDGE_CURVE('',#1753,#1754,#1131,.T.);
#2118=EDGE_CURVE('',#1754,#1754,#1505,.T.);
#2119=EDGE_CURVE('',#1755,#1755,#1506,.T.);
#2120=EDGE_CURVE('',#1755,#1756,#1132,.T.);
#2121=EDGE_CURVE('',#1756,#1756,#1507,.T.);
#2122=EDGE_CURVE('',#1757,#1757,#1508,.T.);
#2123=EDGE_CURVE('',#1757,#1758,#1133,.T.);
#2124=EDGE_CURVE('',#1758,#1758,#1509,.T.);
#2125=EDGE_CURVE('',#1759,#1759,#1510,.T.);
#2126=EDGE_CURVE('',#1759,#1760,#1134,.T.);
#2127=EDGE_CURVE('',#1760,#1760,#1511,.T.);
#2128=EDGE_CURVE('',#1761,#1761,#1512,.T.);
#2129=EDGE_CURVE('',#1761,#1762,#1135,.T.);
#2130=EDGE_CURVE('',#1762,#1762,#1513,.T.);
#2131=EDGE_CURVE('',#1763,#1763,#1514,.T.);
#2132=EDGE_CURVE('',#1763,#1764,#1136,.T.);
#2133=EDGE_CURVE('',#1764,#1764,#1515,.T.);
#2134=EDGE_CURVE('',#1765,#1765,#1516,.T.);
#2135=EDGE_CURVE('',#1766,#1766,#1517,.T.);
#2136=EDGE_CURVE('',#1766,#1765,#1137,.T.);
#2137=EDGE_CURVE('',#1767,#1767,#1518,.T.);
#2138=EDGE_CURVE('',#1767,#1766,#1138,.T.);
#2139=EDGE_CURVE('',#1768,#1768,#1519,.T.);
#2140=EDGE_CURVE('',#1768,#1767,#1139,.T.);
#2141=EDGE_CURVE('',#1769,#1769,#1520,.T.);
#2142=EDGE_CURVE('',#1770,#1770,#1521,.F.);
#2143=EDGE_CURVE('',#1770,#1769,#1140,.T.);
#2144=EDGE_CURVE('',#1771,#1771,#1522,.F.);
#2145=EDGE_CURVE('',#1771,#1770,#1141,.T.);
#2146=EDGE_CURVE('',#1772,#1772,#1523,.T.);
#2147=EDGE_CURVE('',#1772,#1771,#1142,.T.);
#2148=EDGE_CURVE('',#1773,#1774,#1143,.T.);
#2149=EDGE_CURVE('',#1774,#1775,#1144,.T.);
#2150=EDGE_CURVE('',#1775,#1776,#1145,.T.);
#2151=EDGE_CURVE('',#1773,#1776,#1146,.T.);
#2152=EDGE_CURVE('',#1774,#1777,#1147,.T.);
#2153=EDGE_CURVE('',#1777,#1778,#1148,.T.);
#2154=EDGE_CURVE('',#1778,#1775,#1149,.T.);
#2155=EDGE_CURVE('',#1777,#1779,#1150,.T.);
#2156=EDGE_CURVE('',#1779,#1780,#1151,.T.);
#2157=EDGE_CURVE('',#1780,#1778,#1152,.T.);
#2158=EDGE_CURVE('',#1779,#1781,#1153,.T.);
#2159=EDGE_CURVE('',#1781,#1782,#1154,.T.);
#2160=EDGE_CURVE('',#1782,#1780,#1155,.T.);
#2161=EDGE_CURVE('',#1781,#1783,#1156,.T.);
#2162=EDGE_CURVE('',#1783,#1784,#1157,.T.);
#2163=EDGE_CURVE('',#1784,#1782,#1158,.T.);
#2164=EDGE_CURVE('',#1783,#1773,#1159,.T.);
#2165=EDGE_CURVE('',#1776,#1784,#1160,.T.);
#2166=ORIENTED_EDGE('',*,*,#1785,.F.);
#2167=ORIENTED_EDGE('',*,*,#1786,.T.);
#2168=ORIENTED_EDGE('',*,*,#1787,.F.);
#2169=ORIENTED_EDGE('',*,*,#1786,.F.);
#2170=ORIENTED_EDGE('',*,*,#1788,.F.);
#2171=ORIENTED_EDGE('',*,*,#1789,.T.);
#2172=ORIENTED_EDGE('',*,*,#1790,.F.);
#2173=ORIENTED_EDGE('',*,*,#1789,.F.);
#2174=ORIENTED_EDGE('',*,*,#1791,.F.);
#2175=ORIENTED_EDGE('',*,*,#1792,.T.);
#2176=ORIENTED_EDGE('',*,*,#1793,.F.);
#2177=ORIENTED_EDGE('',*,*,#1792,.F.);
#2178=ORIENTED_EDGE('',*,*,#1794,.F.);
#2179=ORIENTED_EDGE('',*,*,#1795,.T.);
#2180=ORIENTED_EDGE('',*,*,#1796,.F.);
#2181=ORIENTED_EDGE('',*,*,#1797,.F.);
#2182=ORIENTED_EDGE('',*,*,#1787,.T.);
#2183=ORIENTED_EDGE('',*,*,#1790,.T.);
#2184=ORIENTED_EDGE('',*,*,#1798,.F.);
#2185=ORIENTED_EDGE('',*,*,#1799,.F.);
#2186=ORIENTED_EDGE('',*,*,#1800,.F.);
#2187=ORIENTED_EDGE('',*,*,#1801,.F.);
#2188=ORIENTED_EDGE('',*,*,#1802,.F.);
#2189=ORIENTED_EDGE('',*,*,#1797,.T.);
#2190=ORIENTED_EDGE('',*,*,#1803,.F.);
#2191=ORIENTED_EDGE('',*,*,#1804,.F.);
#2192=ORIENTED_EDGE('',*,*,#1805,.F.);
#2193=ORIENTED_EDGE('',*,*,#1806,.T.);
#2194=ORIENTED_EDGE('',*,*,#1807,.F.);
#2195=ORIENTED_EDGE('',*,*,#1795,.F.);
#2196=ORIENTED_EDGE('',*,*,#1796,.T.);
#2197=ORIENTED_EDGE('',*,*,#1807,.T.);
#2198=ORIENTED_EDGE('',*,*,#1808,.T.);
#2199=ORIENTED_EDGE('',*,*,#1803,.T.);
#2200=ORIENTED_EDGE('',*,*,#1794,.T.);
#2201=ORIENTED_EDGE('',*,*,#1802,.T.);
#2202=ORIENTED_EDGE('',*,*,#1809,.T.);
#2203=ORIENTED_EDGE('',*,*,#1805,.T.);
#2204=ORIENTED_EDGE('',*,*,#1800,.T.);
#2205=ORIENTED_EDGE('',*,*,#1810,.T.);
#2206=ORIENTED_EDGE('',*,*,#1811,.F.);
#2207=ORIENTED_EDGE('',*,*,#1812,.F.);
#2208=ORIENTED_EDGE('',*,*,#1791,.T.);
#2209=ORIENTED_EDGE('',*,*,#1799,.T.);
#2210=ORIENTED_EDGE('',*,*,#1813,.T.);
#2211=ORIENTED_EDGE('',*,*,#1814,.F.);
#2212=ORIENTED_EDGE('',*,*,#1810,.F.);
#2213=ORIENTED_EDGE('',*,*,#1798,.T.);
#2214=ORIENTED_EDGE('',*,*,#1815,.T.);
#2215=ORIENTED_EDGE('',*,*,#1816,.F.);
#2216=ORIENTED_EDGE('',*,*,#1813,.F.);
#2217=ORIENTED_EDGE('',*,*,#1793,.T.);
#2218=ORIENTED_EDGE('',*,*,#1801,.T.);
#2219=ORIENTED_EDGE('',*,*,#1812,.T.);
#2220=ORIENTED_EDGE('',*,*,#1817,.F.);
#2221=ORIENTED_EDGE('',*,*,#1815,.F.);
#2222=ORIENTED_EDGE('',*,*,#1817,.T.);
#2223=ORIENTED_EDGE('',*,*,#1811,.T.);
#2224=ORIENTED_EDGE('',*,*,#1814,.T.);
#2225=ORIENTED_EDGE('',*,*,#1816,.T.);
#2226=ORIENTED_EDGE('',*,*,#1809,.F.);
#2227=ORIENTED_EDGE('',*,*,#1804,.T.);
#2228=ORIENTED_EDGE('',*,*,#1808,.F.);
#2229=ORIENTED_EDGE('',*,*,#1806,.F.);
#2230=ORIENTED_EDGE('',*,*,#1785,.T.);
#2231=ORIENTED_EDGE('',*,*,#1788,.T.);
#2232=ORIENTED_EDGE('',*,*,#1818,.F.);
#2233=ORIENTED_EDGE('',*,*,#1819,.T.);
#2234=ORIENTED_EDGE('',*,*,#1820,.F.);
#2235=ORIENTED_EDGE('',*,*,#1819,.F.);
#2236=ORIENTED_EDGE('',*,*,#1821,.F.);
#2237=ORIENTED_EDGE('',*,*,#1822,.T.);
#2238=ORIENTED_EDGE('',*,*,#1823,.F.);
#2239=ORIENTED_EDGE('',*,*,#1822,.F.);
#2240=ORIENTED_EDGE('',*,*,#1824,.F.);
#2241=ORIENTED_EDGE('',*,*,#1825,.T.);
#2242=ORIENTED_EDGE('',*,*,#1826,.F.);
#2243=ORIENTED_EDGE('',*,*,#1825,.F.);
#2244=ORIENTED_EDGE('',*,*,#1827,.F.);
#2245=ORIENTED_EDGE('',*,*,#1828,.T.);
#2246=ORIENTED_EDGE('',*,*,#1829,.F.);
#2247=ORIENTED_EDGE('',*,*,#1830,.F.);
#2248=ORIENTED_EDGE('',*,*,#1820,.T.);
#2249=ORIENTED_EDGE('',*,*,#1823,.T.);
#2250=ORIENTED_EDGE('',*,*,#1831,.F.);
#2251=ORIENTED_EDGE('',*,*,#1832,.F.);
#2252=ORIENTED_EDGE('',*,*,#1833,.F.);
#2253=ORIENTED_EDGE('',*,*,#1834,.F.);
#2254=ORIENTED_EDGE('',*,*,#1835,.F.);
#2255=ORIENTED_EDGE('',*,*,#1830,.T.);
#2256=ORIENTED_EDGE('',*,*,#1836,.F.);
#2257=ORIENTED_EDGE('',*,*,#1837,.F.);
#2258=ORIENTED_EDGE('',*,*,#1838,.F.);
#2259=ORIENTED_EDGE('',*,*,#1839,.T.);
#2260=ORIENTED_EDGE('',*,*,#1840,.F.);
#2261=ORIENTED_EDGE('',*,*,#1828,.F.);
#2262=ORIENTED_EDGE('',*,*,#1829,.T.);
#2263=ORIENTED_EDGE('',*,*,#1840,.T.);
#2264=ORIENTED_EDGE('',*,*,#1841,.T.);
#2265=ORIENTED_EDGE('',*,*,#1836,.T.);
#2266=ORIENTED_EDGE('',*,*,#1827,.T.);
#2267=ORIENTED_EDGE('',*,*,#1835,.T.);
#2268=ORIENTED_EDGE('',*,*,#1842,.T.);
#2269=ORIENTED_EDGE('',*,*,#1838,.T.);
#2270=ORIENTED_EDGE('',*,*,#1833,.T.);
#2271=ORIENTED_EDGE('',*,*,#1843,.T.);
#2272=ORIENTED_EDGE('',*,*,#1844,.F.);
#2273=ORIENTED_EDGE('',*,*,#1845,.F.);
#2274=ORIENTED_EDGE('',*,*,#1824,.T.);
#2275=ORIENTED_EDGE('',*,*,#1832,.T.);
#2276=ORIENTED_EDGE('',*,*,#1846,.T.);
#2277=ORIENTED_EDGE('',*,*,#1847,.F.);
#2278=ORIENTED_EDGE('',*,*,#1843,.F.);
#2279=ORIENTED_EDGE('',*,*,#1831,.T.);
#2280=ORIENTED_EDGE('',*,*,#1848,.T.);
#2281=ORIENTED_EDGE('',*,*,#1849,.F.);
#2282=ORIENTED_EDGE('',*,*,#1846,.F.);
#2283=ORIENTED_EDGE('',*,*,#1826,.T.);
#2284=ORIENTED_EDGE('',*,*,#1834,.T.);
#2285=ORIENTED_EDGE('',*,*,#1845,.T.);
#2286=ORIENTED_EDGE('',*,*,#1850,.F.);
#2287=ORIENTED_EDGE('',*,*,#1848,.F.);
#2288=ORIENTED_EDGE('',*,*,#1850,.T.);
#2289=ORIENTED_EDGE('',*,*,#1844,.T.);
#2290=ORIENTED_EDGE('',*,*,#1847,.T.);
#2291=ORIENTED_EDGE('',*,*,#1849,.T.);
#2292=ORIENTED_EDGE('',*,*,#1842,.F.);
#2293=ORIENTED_EDGE('',*,*,#1837,.T.);
#2294=ORIENTED_EDGE('',*,*,#1841,.F.);
#2295=ORIENTED_EDGE('',*,*,#1839,.F.);
#2296=ORIENTED_EDGE('',*,*,#1818,.T.);
#2297=ORIENTED_EDGE('',*,*,#1821,.T.);
#2298=ORIENTED_EDGE('',*,*,#1851,.F.);
#2299=ORIENTED_EDGE('',*,*,#1852,.T.);
#2300=ORIENTED_EDGE('',*,*,#1853,.F.);
#2301=ORIENTED_EDGE('',*,*,#1852,.F.);
#2302=ORIENTED_EDGE('',*,*,#1851,.T.);
#2303=ORIENTED_EDGE('',*,*,#1854,.F.);
#2304=ORIENTED_EDGE('',*,*,#1855,.T.);
#2305=ORIENTED_EDGE('',*,*,#1856,.T.);
#2306=ORIENTED_EDGE('',*,*,#1855,.F.);
#2307=ORIENTED_EDGE('',*,*,#1856,.F.);
#2308=ORIENTED_EDGE('',*,*,#1857,.T.);
#2309=ORIENTED_EDGE('',*,*,#1858,.F.);
#2310=ORIENTED_EDGE('',*,*,#1859,.F.);
#2311=ORIENTED_EDGE('',*,*,#1860,.F.);
#2312=ORIENTED_EDGE('',*,*,#1857,.F.);
#2313=ORIENTED_EDGE('',*,*,#1861,.T.);
#2314=ORIENTED_EDGE('',*,*,#1859,.T.);
#2315=ORIENTED_EDGE('',*,*,#1861,.F.);
#2316=ORIENTED_EDGE('',*,*,#1860,.T.);
#2317=ORIENTED_EDGE('',*,*,#1862,.T.);
#2318=ORIENTED_EDGE('',*,*,#1863,.T.);
#2319=ORIENTED_EDGE('',*,*,#1862,.F.);
#2320=ORIENTED_EDGE('',*,*,#1864,.F.);
#2321=ORIENTED_EDGE('',*,*,#1865,.T.);
#2322=ORIENTED_EDGE('',*,*,#1858,.T.);
#2323=ORIENTED_EDGE('',*,*,#1865,.F.);
#2324=ORIENTED_EDGE('',*,*,#1864,.T.);
#2325=ORIENTED_EDGE('',*,*,#1853,.T.);
#2326=ORIENTED_EDGE('',*,*,#1863,.F.);
#2327=ORIENTED_EDGE('',*,*,#1854,.T.);
#2328=ORIENTED_EDGE('',*,*,#1866,.F.);
#2329=ORIENTED_EDGE('',*,*,#1867,.T.);
#2330=ORIENTED_EDGE('',*,*,#1868,.T.);
#2331=ORIENTED_EDGE('',*,*,#1867,.F.);
#2332=ORIENTED_EDGE('',*,*,#1869,.F.);
#2333=ORIENTED_EDGE('',*,*,#1870,.T.);
#2334=ORIENTED_EDGE('',*,*,#1871,.T.);
#2335=ORIENTED_EDGE('',*,*,#1870,.F.);
#2336=ORIENTED_EDGE('',*,*,#1869,.T.);
#2337=ORIENTED_EDGE('',*,*,#1866,.T.);
#2338=ORIENTED_EDGE('',*,*,#1871,.F.);
#2339=ORIENTED_EDGE('',*,*,#1868,.F.);
#2340=ORIENTED_EDGE('',*,*,#1872,.F.);
#2341=ORIENTED_EDGE('',*,*,#1873,.T.);
#2342=ORIENTED_EDGE('',*,*,#1874,.T.);
#2343=ORIENTED_EDGE('',*,*,#1873,.F.);
#2344=ORIENTED_EDGE('',*,*,#1875,.F.);
#2345=ORIENTED_EDGE('',*,*,#1876,.T.);
#2346=ORIENTED_EDGE('',*,*,#1877,.T.);
#2347=ORIENTED_EDGE('',*,*,#1876,.F.);
#2348=ORIENTED_EDGE('',*,*,#1875,.T.);
#2349=ORIENTED_EDGE('',*,*,#1872,.T.);
#2350=ORIENTED_EDGE('',*,*,#1877,.F.);
#2351=ORIENTED_EDGE('',*,*,#1874,.F.);
#2352=ORIENTED_EDGE('',*,*,#1878,.F.);
#2353=ORIENTED_EDGE('',*,*,#1879,.T.);
#2354=ORIENTED_EDGE('',*,*,#1880,.F.);
#2355=ORIENTED_EDGE('',*,*,#1879,.F.);
#2356=ORIENTED_EDGE('',*,*,#1881,.F.);
#2357=ORIENTED_EDGE('',*,*,#1882,.T.);
#2358=ORIENTED_EDGE('',*,*,#1883,.F.);
#2359=ORIENTED_EDGE('',*,*,#1882,.F.);
#2360=ORIENTED_EDGE('',*,*,#1884,.F.);
#2361=ORIENTED_EDGE('',*,*,#1885,.T.);
#2362=ORIENTED_EDGE('',*,*,#1886,.F.);
#2363=ORIENTED_EDGE('',*,*,#1885,.F.);
#2364=ORIENTED_EDGE('',*,*,#1887,.F.);
#2365=ORIENTED_EDGE('',*,*,#1888,.T.);
#2366=ORIENTED_EDGE('',*,*,#1889,.F.);
#2367=ORIENTED_EDGE('',*,*,#1888,.F.);
#2368=ORIENTED_EDGE('',*,*,#1890,.T.);
#2369=ORIENTED_EDGE('',*,*,#1891,.T.);
#2370=ORIENTED_EDGE('',*,*,#1892,.F.);
#2371=ORIENTED_EDGE('',*,*,#1893,.F.);
#2372=ORIENTED_EDGE('',*,*,#1894,.T.);
#2373=ORIENTED_EDGE('',*,*,#1893,.T.);
#2374=ORIENTED_EDGE('',*,*,#1895,.F.);
#2375=ORIENTED_EDGE('',*,*,#1896,.F.);
#2376=ORIENTED_EDGE('',*,*,#1897,.T.);
#2377=ORIENTED_EDGE('',*,*,#1896,.T.);
#2378=ORIENTED_EDGE('',*,*,#1898,.F.);
#2379=ORIENTED_EDGE('',*,*,#1899,.F.);
#2380=ORIENTED_EDGE('',*,*,#1900,.T.);
#2381=ORIENTED_EDGE('',*,*,#1899,.T.);
#2382=ORIENTED_EDGE('',*,*,#1901,.F.);
#2383=ORIENTED_EDGE('',*,*,#1891,.F.);
#2384=ORIENTED_EDGE('',*,*,#1901,.T.);
#2385=ORIENTED_EDGE('',*,*,#1898,.T.);
#2386=ORIENTED_EDGE('',*,*,#1895,.T.);
#2387=ORIENTED_EDGE('',*,*,#1892,.T.);
#2388=ORIENTED_EDGE('',*,*,#1880,.T.);
#2389=ORIENTED_EDGE('',*,*,#1883,.T.);
#2390=ORIENTED_EDGE('',*,*,#1886,.T.);
#2391=ORIENTED_EDGE('',*,*,#1889,.T.);
#2392=ORIENTED_EDGE('',*,*,#1900,.F.);
#2393=ORIENTED_EDGE('',*,*,#1890,.F.);
#2394=ORIENTED_EDGE('',*,*,#1894,.F.);
#2395=ORIENTED_EDGE('',*,*,#1897,.F.);
#2396=ORIENTED_EDGE('',*,*,#1878,.T.);
#2397=ORIENTED_EDGE('',*,*,#1881,.T.);
#2398=ORIENTED_EDGE('',*,*,#1884,.T.);
#2399=ORIENTED_EDGE('',*,*,#1887,.T.);
#2400=ORIENTED_EDGE('',*,*,#1902,.T.);
#2401=ORIENTED_EDGE('',*,*,#1903,.T.);
#2402=ORIENTED_EDGE('',*,*,#1904,.F.);
#2403=ORIENTED_EDGE('',*,*,#1905,.F.);
#2404=ORIENTED_EDGE('',*,*,#1906,.T.);
#2405=ORIENTED_EDGE('',*,*,#1905,.T.);
#2406=ORIENTED_EDGE('',*,*,#1907,.F.);
#2407=ORIENTED_EDGE('',*,*,#1908,.F.);
#2408=ORIENTED_EDGE('',*,*,#1909,.T.);
#2409=ORIENTED_EDGE('',*,*,#1908,.T.);
#2410=ORIENTED_EDGE('',*,*,#1910,.F.);
#2411=ORIENTED_EDGE('',*,*,#1911,.F.);
#2412=ORIENTED_EDGE('',*,*,#1912,.T.);
#2413=ORIENTED_EDGE('',*,*,#1911,.T.);
#2414=ORIENTED_EDGE('',*,*,#1913,.F.);
#2415=ORIENTED_EDGE('',*,*,#1903,.F.);
#2416=ORIENTED_EDGE('',*,*,#1913,.T.);
#2417=ORIENTED_EDGE('',*,*,#1910,.T.);
#2418=ORIENTED_EDGE('',*,*,#1907,.T.);
#2419=ORIENTED_EDGE('',*,*,#1904,.T.);
#2420=ORIENTED_EDGE('',*,*,#1912,.F.);
#2421=ORIENTED_EDGE('',*,*,#1902,.F.);
#2422=ORIENTED_EDGE('',*,*,#1906,.F.);
#2423=ORIENTED_EDGE('',*,*,#1909,.F.);
#2424=ORIENTED_EDGE('',*,*,#1914,.F.);
#2425=ORIENTED_EDGE('',*,*,#1915,.T.);
#2426=ORIENTED_EDGE('',*,*,#1916,.T.);
#2427=ORIENTED_EDGE('',*,*,#1915,.F.);
#2428=ORIENTED_EDGE('',*,*,#1917,.F.);
#2429=ORIENTED_EDGE('',*,*,#1918,.T.);
#2430=ORIENTED_EDGE('',*,*,#1919,.T.);
#2431=ORIENTED_EDGE('',*,*,#1918,.F.);
#2432=ORIENTED_EDGE('',*,*,#1917,.T.);
#2433=ORIENTED_EDGE('',*,*,#1914,.T.);
#2434=ORIENTED_EDGE('',*,*,#1919,.F.);
#2435=ORIENTED_EDGE('',*,*,#1916,.F.);
#2436=ORIENTED_EDGE('',*,*,#1920,.T.);
#2437=ORIENTED_EDGE('',*,*,#1921,.T.);
#2438=ORIENTED_EDGE('',*,*,#1922,.T.);
#2439=ORIENTED_EDGE('',*,*,#1923,.F.);
#2440=ORIENTED_EDGE('',*,*,#1924,.T.);
#2441=ORIENTED_EDGE('',*,*,#1925,.T.);
#2442=ORIENTED_EDGE('',*,*,#1926,.T.);
#2443=ORIENTED_EDGE('',*,*,#1921,.F.);
#2444=ORIENTED_EDGE('',*,*,#1927,.T.);
#2445=ORIENTED_EDGE('',*,*,#1928,.T.);
#2446=ORIENTED_EDGE('',*,*,#1929,.T.);
#2447=ORIENTED_EDGE('',*,*,#1925,.F.);
#2448=ORIENTED_EDGE('',*,*,#1930,.T.);
#2449=ORIENTED_EDGE('',*,*,#1931,.T.);
#2450=ORIENTED_EDGE('',*,*,#1932,.T.);
#2451=ORIENTED_EDGE('',*,*,#1928,.F.);
#2452=ORIENTED_EDGE('',*,*,#1933,.T.);
#2453=ORIENTED_EDGE('',*,*,#1934,.T.);
#2454=ORIENTED_EDGE('',*,*,#1935,.T.);
#2455=ORIENTED_EDGE('',*,*,#1931,.F.);
#2456=ORIENTED_EDGE('',*,*,#1936,.T.);
#2457=ORIENTED_EDGE('',*,*,#1923,.T.);
#2458=ORIENTED_EDGE('',*,*,#1937,.T.);
#2459=ORIENTED_EDGE('',*,*,#1934,.F.);
#2460=ORIENTED_EDGE('',*,*,#1936,.F.);
#2461=ORIENTED_EDGE('',*,*,#1933,.F.);
#2462=ORIENTED_EDGE('',*,*,#1930,.F.);
#2463=ORIENTED_EDGE('',*,*,#1927,.F.);
#2464=ORIENTED_EDGE('',*,*,#1924,.F.);
#2465=ORIENTED_EDGE('',*,*,#1920,.F.);
#2466=ORIENTED_EDGE('',*,*,#1937,.F.);
#2467=ORIENTED_EDGE('',*,*,#1922,.F.);
#2468=ORIENTED_EDGE('',*,*,#1926,.F.);
#2469=ORIENTED_EDGE('',*,*,#1929,.F.);
#2470=ORIENTED_EDGE('',*,*,#1932,.F.);
#2471=ORIENTED_EDGE('',*,*,#1935,.F.);
#2472=ORIENTED_EDGE('',*,*,#1938,.F.);
#2473=ORIENTED_EDGE('',*,*,#1939,.F.);
#2474=ORIENTED_EDGE('',*,*,#1940,.F.);
#2475=ORIENTED_EDGE('',*,*,#1941,.T.);
#2476=ORIENTED_EDGE('',*,*,#1939,.T.);
#2477=ORIENTED_EDGE('',*,*,#1941,.F.);
#2478=ORIENTED_EDGE('',*,*,#1942,.F.);
#2479=ORIENTED_EDGE('',*,*,#1943,.T.);
#2480=ORIENTED_EDGE('',*,*,#1940,.T.);
#2481=ORIENTED_EDGE('',*,*,#1943,.F.);
#2482=ORIENTED_EDGE('',*,*,#1944,.F.);
#2483=ORIENTED_EDGE('',*,*,#1945,.T.);
#2484=ORIENTED_EDGE('',*,*,#1942,.T.);
#2485=ORIENTED_EDGE('',*,*,#1945,.F.);
#2486=ORIENTED_EDGE('',*,*,#1944,.T.);
#2487=ORIENTED_EDGE('',*,*,#1946,.F.);
#2488=ORIENTED_EDGE('',*,*,#1947,.F.);
#2489=ORIENTED_EDGE('',*,*,#1948,.T.);
#2490=ORIENTED_EDGE('',*,*,#1946,.T.);
#2491=ORIENTED_EDGE('',*,*,#1948,.F.);
#2492=ORIENTED_EDGE('',*,*,#1938,.T.);
#2493=ORIENTED_EDGE('',*,*,#1949,.T.);
#2494=ORIENTED_EDGE('',*,*,#1947,.T.);
#2495=ORIENTED_EDGE('',*,*,#1949,.F.);
#2496=ORIENTED_EDGE('',*,*,#1950,.F.);
#2497=ORIENTED_EDGE('',*,*,#1951,.T.);
#2498=ORIENTED_EDGE('',*,*,#1952,.T.);
#2499=ORIENTED_EDGE('',*,*,#1951,.F.);
#2500=ORIENTED_EDGE('',*,*,#1953,.F.);
#2501=ORIENTED_EDGE('',*,*,#1954,.T.);
#2502=ORIENTED_EDGE('',*,*,#1955,.T.);
#2503=ORIENTED_EDGE('',*,*,#1954,.F.);
#2504=ORIENTED_EDGE('',*,*,#1953,.T.);
#2505=ORIENTED_EDGE('',*,*,#1950,.T.);
#2506=ORIENTED_EDGE('',*,*,#1955,.F.);
#2507=ORIENTED_EDGE('',*,*,#1952,.F.);
#2508=ORIENTED_EDGE('',*,*,#1956,.F.);
#2509=ORIENTED_EDGE('',*,*,#1957,.T.);
#2510=ORIENTED_EDGE('',*,*,#1958,.T.);
#2511=ORIENTED_EDGE('',*,*,#1957,.F.);
#2512=ORIENTED_EDGE('',*,*,#1959,.F.);
#2513=ORIENTED_EDGE('',*,*,#1960,.T.);
#2514=ORIENTED_EDGE('',*,*,#1961,.T.);
#2515=ORIENTED_EDGE('',*,*,#1960,.F.);
#2516=ORIENTED_EDGE('',*,*,#1959,.T.);
#2517=ORIENTED_EDGE('',*,*,#1956,.T.);
#2518=ORIENTED_EDGE('',*,*,#1961,.F.);
#2519=ORIENTED_EDGE('',*,*,#1958,.F.);
#2520=ORIENTED_EDGE('',*,*,#1962,.F.);
#2521=ORIENTED_EDGE('',*,*,#1963,.F.);
#2522=ORIENTED_EDGE('',*,*,#1964,.T.);
#2523=ORIENTED_EDGE('',*,*,#1965,.F.);
#2524=ORIENTED_EDGE('',*,*,#1966,.F.);
#2525=ORIENTED_EDGE('',*,*,#1964,.F.);
#2526=ORIENTED_EDGE('',*,*,#1965,.T.);
#2527=ORIENTED_EDGE('',*,*,#1966,.T.);
#2528=ORIENTED_EDGE('',*,*,#1967,.T.);
#2529=ORIENTED_EDGE('',*,*,#1968,.T.);
#2530=ORIENTED_EDGE('',*,*,#1967,.F.);
#2531=ORIENTED_EDGE('',*,*,#1969,.T.);
#2532=ORIENTED_EDGE('',*,*,#1970,.T.);
#2533=ORIENTED_EDGE('',*,*,#1971,.F.);
#2534=ORIENTED_EDGE('',*,*,#1970,.F.);
#2535=ORIENTED_EDGE('',*,*,#1971,.T.);
#2536=ORIENTED_EDGE('',*,*,#1972,.T.);
#2537=ORIENTED_EDGE('',*,*,#1973,.F.);
#2538=ORIENTED_EDGE('',*,*,#1972,.F.);
#2539=ORIENTED_EDGE('',*,*,#1968,.F.);
#2540=ORIENTED_EDGE('',*,*,#1973,.T.);
#2541=ORIENTED_EDGE('',*,*,#1974,.F.);
#2542=ORIENTED_EDGE('',*,*,#1975,.T.);
#2543=ORIENTED_EDGE('',*,*,#1962,.T.);
#2544=ORIENTED_EDGE('',*,*,#1963,.T.);
#2545=ORIENTED_EDGE('',*,*,#1975,.F.);
#2546=ORIENTED_EDGE('',*,*,#1974,.T.);
#2547=ORIENTED_EDGE('',*,*,#1976,.F.);
#2548=ORIENTED_EDGE('',*,*,#1976,.T.);
#2549=ORIENTED_EDGE('',*,*,#1977,.T.);
#2550=ORIENTED_EDGE('',*,*,#1969,.F.);
#2551=ORIENTED_EDGE('',*,*,#1977,.F.);
#2552=ORIENTED_EDGE('',*,*,#1978,.F.);
#2553=ORIENTED_EDGE('',*,*,#1979,.F.);
#2554=ORIENTED_EDGE('',*,*,#1980,.T.);
#2555=ORIENTED_EDGE('',*,*,#1981,.F.);
#2556=ORIENTED_EDGE('',*,*,#1982,.F.);
#2557=ORIENTED_EDGE('',*,*,#1980,.F.);
#2558=ORIENTED_EDGE('',*,*,#1983,.T.);
#2559=ORIENTED_EDGE('',*,*,#1984,.T.);
#2560=ORIENTED_EDGE('',*,*,#1981,.T.);
#2561=ORIENTED_EDGE('',*,*,#1982,.T.);
#2562=ORIENTED_EDGE('',*,*,#1984,.F.);
#2563=ORIENTED_EDGE('',*,*,#1985,.F.);
#2564=ORIENTED_EDGE('',*,*,#1986,.T.);
#2565=ORIENTED_EDGE('',*,*,#1987,.F.);
#2566=ORIENTED_EDGE('',*,*,#1988,.T.);
#2567=ORIENTED_EDGE('',*,*,#1985,.T.);
#2568=ORIENTED_EDGE('',*,*,#1988,.F.);
#2569=ORIENTED_EDGE('',*,*,#1989,.F.);
#2570=ORIENTED_EDGE('',*,*,#1990,.T.);
#2571=ORIENTED_EDGE('',*,*,#1987,.T.);
#2572=ORIENTED_EDGE('',*,*,#1990,.F.);
#2573=ORIENTED_EDGE('',*,*,#1991,.F.);
#2574=ORIENTED_EDGE('',*,*,#1992,.T.);
#2575=ORIENTED_EDGE('',*,*,#1989,.T.);
#2576=ORIENTED_EDGE('',*,*,#1992,.F.);
#2577=ORIENTED_EDGE('',*,*,#1991,.T.);
#2578=ORIENTED_EDGE('',*,*,#1983,.F.);
#2579=ORIENTED_EDGE('',*,*,#1978,.T.);
#2580=ORIENTED_EDGE('',*,*,#1979,.T.);
#2581=ORIENTED_EDGE('',*,*,#1993,.T.);
#2582=ORIENTED_EDGE('',*,*,#1986,.F.);
#2583=ORIENTED_EDGE('',*,*,#1993,.F.);
#2584=ORIENTED_EDGE('',*,*,#1994,.T.);
#2585=ORIENTED_EDGE('',*,*,#1994,.F.);
#2586=ORIENTED_EDGE('',*,*,#1995,.T.);
#2587=ORIENTED_EDGE('',*,*,#1995,.F.);
#2588=ORIENTED_EDGE('',*,*,#1996,.T.);
#2589=ORIENTED_EDGE('',*,*,#1996,.F.);
#2590=ORIENTED_EDGE('',*,*,#1997,.T.);
#2591=ORIENTED_EDGE('',*,*,#1997,.F.);
#2592=ORIENTED_EDGE('',*,*,#1998,.T.);
#2593=ORIENTED_EDGE('',*,*,#1998,.F.);
#2594=ORIENTED_EDGE('',*,*,#1999,.T.);
#2595=ORIENTED_EDGE('',*,*,#1999,.F.);
#2596=ORIENTED_EDGE('',*,*,#2000,.T.);
#2597=ORIENTED_EDGE('',*,*,#2000,.F.);
#2598=ORIENTED_EDGE('',*,*,#2001,.T.);
#2599=ORIENTED_EDGE('',*,*,#2001,.F.);
#2600=ORIENTED_EDGE('',*,*,#2002,.F.);
#2601=ORIENTED_EDGE('',*,*,#2003,.F.);
#2602=ORIENTED_EDGE('',*,*,#2004,.F.);
#2603=ORIENTED_EDGE('',*,*,#2005,.F.);
#2604=ORIENTED_EDGE('',*,*,#2004,.T.);
#2605=ORIENTED_EDGE('',*,*,#2006,.F.);
#2606=ORIENTED_EDGE('',*,*,#2007,.T.);
#2607=ORIENTED_EDGE('',*,*,#2008,.F.);
#2608=ORIENTED_EDGE('',*,*,#2009,.T.);
#2609=ORIENTED_EDGE('',*,*,#2010,.F.);
#2610=ORIENTED_EDGE('',*,*,#2011,.T.);
#2611=ORIENTED_EDGE('',*,*,#2012,.T.);
#2612=ORIENTED_EDGE('',*,*,#2013,.F.);
#2613=ORIENTED_EDGE('',*,*,#2012,.F.);
#2614=ORIENTED_EDGE('',*,*,#2014,.T.);
#2615=ORIENTED_EDGE('',*,*,#2015,.F.);
#2616=ORIENTED_EDGE('',*,*,#2016,.T.);
#2617=ORIENTED_EDGE('',*,*,#2017,.F.);
#2618=ORIENTED_EDGE('',*,*,#2018,.T.);
#2619=ORIENTED_EDGE('',*,*,#2019,.F.);
#2620=ORIENTED_EDGE('',*,*,#2020,.T.);
#2621=ORIENTED_EDGE('',*,*,#2021,.F.);
#2622=ORIENTED_EDGE('',*,*,#2022,.T.);
#2623=ORIENTED_EDGE('',*,*,#2023,.F.);
#2624=ORIENTED_EDGE('',*,*,#2003,.T.);
#2625=ORIENTED_EDGE('',*,*,#2024,.T.);
#2626=ORIENTED_EDGE('',*,*,#2025,.T.);
#2627=ORIENTED_EDGE('',*,*,#2006,.T.);
#2628=ORIENTED_EDGE('',*,*,#2026,.F.);
#2629=ORIENTED_EDGE('',*,*,#2027,.F.);
#2630=ORIENTED_EDGE('',*,*,#2007,.F.);
#2631=ORIENTED_EDGE('',*,*,#2025,.F.);
#2632=ORIENTED_EDGE('',*,*,#2027,.T.);
#2633=ORIENTED_EDGE('',*,*,#2028,.T.);
#2634=ORIENTED_EDGE('',*,*,#2029,.T.);
#2635=ORIENTED_EDGE('',*,*,#2008,.T.);
#2636=ORIENTED_EDGE('',*,*,#2030,.F.);
#2637=ORIENTED_EDGE('',*,*,#2031,.F.);
#2638=ORIENTED_EDGE('',*,*,#2009,.F.);
#2639=ORIENTED_EDGE('',*,*,#2029,.F.);
#2640=ORIENTED_EDGE('',*,*,#2031,.T.);
#2641=ORIENTED_EDGE('',*,*,#2032,.T.);
#2642=ORIENTED_EDGE('',*,*,#2033,.T.);
#2643=ORIENTED_EDGE('',*,*,#2010,.T.);
#2644=ORIENTED_EDGE('',*,*,#2034,.F.);
#2645=ORIENTED_EDGE('',*,*,#2035,.F.);
#2646=ORIENTED_EDGE('',*,*,#2014,.F.);
#2647=ORIENTED_EDGE('',*,*,#2011,.F.);
#2648=ORIENTED_EDGE('',*,*,#2033,.F.);
#2649=ORIENTED_EDGE('',*,*,#2036,.F.);
#2650=ORIENTED_EDGE('',*,*,#2035,.T.);
#2651=ORIENTED_EDGE('',*,*,#2037,.T.);
#2652=ORIENTED_EDGE('',*,*,#2038,.T.);
#2653=ORIENTED_EDGE('',*,*,#2015,.T.);
#2654=ORIENTED_EDGE('',*,*,#2039,.F.);
#2655=ORIENTED_EDGE('',*,*,#2040,.F.);
#2656=ORIENTED_EDGE('',*,*,#2016,.F.);
#2657=ORIENTED_EDGE('',*,*,#2038,.F.);
#2658=ORIENTED_EDGE('',*,*,#2040,.T.);
#2659=ORIENTED_EDGE('',*,*,#2041,.T.);
#2660=ORIENTED_EDGE('',*,*,#2042,.T.);
#2661=ORIENTED_EDGE('',*,*,#2017,.T.);
#2662=ORIENTED_EDGE('',*,*,#2043,.F.);
#2663=ORIENTED_EDGE('',*,*,#2044,.F.);
#2664=ORIENTED_EDGE('',*,*,#2018,.F.);
#2665=ORIENTED_EDGE('',*,*,#2042,.F.);
#2666=ORIENTED_EDGE('',*,*,#2044,.T.);
#2667=ORIENTED_EDGE('',*,*,#2045,.T.);
#2668=ORIENTED_EDGE('',*,*,#2046,.T.);
#2669=ORIENTED_EDGE('',*,*,#2019,.T.);
#2670=ORIENTED_EDGE('',*,*,#2020,.F.);
#2671=ORIENTED_EDGE('',*,*,#2046,.F.);
#2672=ORIENTED_EDGE('',*,*,#2047,.F.);
#2673=ORIENTED_EDGE('',*,*,#2048,.F.);
#2674=ORIENTED_EDGE('',*,*,#2049,.F.);
#2675=ORIENTED_EDGE('',*,*,#2050,.T.);
#2676=ORIENTED_EDGE('',*,*,#2036,.T.);
#2677=ORIENTED_EDGE('',*,*,#2032,.F.);
#2678=ORIENTED_EDGE('',*,*,#2030,.T.);
#2679=ORIENTED_EDGE('',*,*,#2028,.F.);
#2680=ORIENTED_EDGE('',*,*,#2026,.T.);
#2681=ORIENTED_EDGE('',*,*,#2024,.F.);
#2682=ORIENTED_EDGE('',*,*,#2002,.T.);
#2683=ORIENTED_EDGE('',*,*,#2051,.F.);
#2684=ORIENTED_EDGE('',*,*,#2052,.T.);
#2685=ORIENTED_EDGE('',*,*,#2053,.F.);
#2686=ORIENTED_EDGE('',*,*,#2047,.T.);
#2687=ORIENTED_EDGE('',*,*,#2045,.F.);
#2688=ORIENTED_EDGE('',*,*,#2043,.T.);
#2689=ORIENTED_EDGE('',*,*,#2041,.F.);
#2690=ORIENTED_EDGE('',*,*,#2039,.T.);
#2691=ORIENTED_EDGE('',*,*,#2037,.F.);
#2692=ORIENTED_EDGE('',*,*,#2034,.T.);
#2693=ORIENTED_EDGE('',*,*,#2050,.F.);
#2694=ORIENTED_EDGE('',*,*,#2005,.T.);
#2695=ORIENTED_EDGE('',*,*,#2023,.T.);
#2696=ORIENTED_EDGE('',*,*,#2054,.T.);
#2697=ORIENTED_EDGE('',*,*,#2051,.T.);
#2698=ORIENTED_EDGE('',*,*,#2022,.F.);
#2699=ORIENTED_EDGE('',*,*,#2055,.F.);
#2700=ORIENTED_EDGE('',*,*,#2052,.F.);
#2701=ORIENTED_EDGE('',*,*,#2054,.F.);
#2702=ORIENTED_EDGE('',*,*,#2013,.T.);
#2703=ORIENTED_EDGE('',*,*,#2049,.T.);
#2704=ORIENTED_EDGE('',*,*,#2048,.T.);
#2705=ORIENTED_EDGE('',*,*,#2053,.T.);
#2706=ORIENTED_EDGE('',*,*,#2055,.T.);
#2707=ORIENTED_EDGE('',*,*,#2021,.T.);
#2708=ORIENTED_EDGE('',*,*,#2056,.F.);
#2709=ORIENTED_EDGE('',*,*,#2057,.T.);
#2710=ORIENTED_EDGE('',*,*,#2058,.F.);
#2711=ORIENTED_EDGE('',*,*,#2059,.T.);
#2712=ORIENTED_EDGE('',*,*,#2056,.T.);
#2713=ORIENTED_EDGE('',*,*,#2059,.F.);
#2714=ORIENTED_EDGE('',*,*,#2058,.T.);
#2715=ORIENTED_EDGE('',*,*,#2060,.F.);
#2716=ORIENTED_EDGE('',*,*,#2060,.T.);
#2717=ORIENTED_EDGE('',*,*,#2061,.T.);
#2718=ORIENTED_EDGE('',*,*,#2057,.F.);
#2719=ORIENTED_EDGE('',*,*,#2061,.F.);
#2720=ORIENTED_EDGE('',*,*,#2062,.F.);
#2721=ORIENTED_EDGE('',*,*,#2063,.T.);
#2722=ORIENTED_EDGE('',*,*,#2064,.F.);
#2723=ORIENTED_EDGE('',*,*,#2065,.T.);
#2724=ORIENTED_EDGE('',*,*,#2062,.T.);
#2725=ORIENTED_EDGE('',*,*,#2065,.F.);
#2726=ORIENTED_EDGE('',*,*,#2064,.T.);
#2727=ORIENTED_EDGE('',*,*,#2066,.F.);
#2728=ORIENTED_EDGE('',*,*,#2066,.T.);
#2729=ORIENTED_EDGE('',*,*,#2067,.T.);
#2730=ORIENTED_EDGE('',*,*,#2063,.F.);
#2731=ORIENTED_EDGE('',*,*,#2067,.F.);
#2732=ORIENTED_EDGE('',*,*,#2068,.F.);
#2733=ORIENTED_EDGE('',*,*,#2069,.T.);
#2734=ORIENTED_EDGE('',*,*,#2070,.F.);
#2735=ORIENTED_EDGE('',*,*,#2069,.F.);
#2736=ORIENTED_EDGE('',*,*,#2071,.F.);
#2737=ORIENTED_EDGE('',*,*,#2072,.T.);
#2738=ORIENTED_EDGE('',*,*,#2073,.F.);
#2739=ORIENTED_EDGE('',*,*,#2072,.F.);
#2740=ORIENTED_EDGE('',*,*,#2074,.F.);
#2741=ORIENTED_EDGE('',*,*,#2075,.T.);
#2742=ORIENTED_EDGE('',*,*,#2076,.F.);
#2743=ORIENTED_EDGE('',*,*,#2075,.F.);
#2744=ORIENTED_EDGE('',*,*,#2077,.F.);
#2745=ORIENTED_EDGE('',*,*,#2078,.T.);
#2746=ORIENTED_EDGE('',*,*,#2079,.F.);
#2747=ORIENTED_EDGE('',*,*,#2078,.F.);
#2748=ORIENTED_EDGE('',*,*,#2080,.F.);
#2749=ORIENTED_EDGE('',*,*,#2081,.T.);
#2750=ORIENTED_EDGE('',*,*,#2082,.T.);
#2751=ORIENTED_EDGE('',*,*,#2081,.F.);
#2752=ORIENTED_EDGE('',*,*,#2083,.F.);
#2753=ORIENTED_EDGE('',*,*,#2082,.F.);
#2754=ORIENTED_EDGE('',*,*,#2083,.T.);
#2755=ORIENTED_EDGE('',*,*,#2084,.T.);
#2756=ORIENTED_EDGE('',*,*,#2085,.T.);
#2757=ORIENTED_EDGE('',*,*,#2084,.F.);
#2758=ORIENTED_EDGE('',*,*,#2086,.F.);
#2759=ORIENTED_EDGE('',*,*,#2087,.T.);
#2760=ORIENTED_EDGE('',*,*,#2088,.T.);
#2761=ORIENTED_EDGE('',*,*,#2087,.F.);
#2762=ORIENTED_EDGE('',*,*,#2086,.T.);
#2763=ORIENTED_EDGE('',*,*,#2080,.T.);
#2764=ORIENTED_EDGE('',*,*,#2079,.T.);
#2765=ORIENTED_EDGE('',*,*,#2076,.T.);
#2766=ORIENTED_EDGE('',*,*,#2073,.T.);
#2767=ORIENTED_EDGE('',*,*,#2070,.T.);
#2768=ORIENTED_EDGE('',*,*,#2088,.F.);
#2769=ORIENTED_EDGE('',*,*,#2085,.F.);
#2770=ORIENTED_EDGE('',*,*,#2077,.T.);
#2771=ORIENTED_EDGE('',*,*,#2074,.T.);
#2772=ORIENTED_EDGE('',*,*,#2071,.T.);
#2773=ORIENTED_EDGE('',*,*,#2068,.T.);
#2774=ORIENTED_EDGE('',*,*,#2089,.F.);
#2775=ORIENTED_EDGE('',*,*,#2090,.T.);
#2776=ORIENTED_EDGE('',*,*,#2091,.F.);
#2777=ORIENTED_EDGE('',*,*,#2090,.F.);
#2778=ORIENTED_EDGE('',*,*,#2092,.F.);
#2779=ORIENTED_EDGE('',*,*,#2093,.T.);
#2780=ORIENTED_EDGE('',*,*,#2094,.F.);
#2781=ORIENTED_EDGE('',*,*,#2093,.F.);
#2782=ORIENTED_EDGE('',*,*,#2095,.F.);
#2783=ORIENTED_EDGE('',*,*,#2096,.T.);
#2784=ORIENTED_EDGE('',*,*,#2097,.F.);
#2785=ORIENTED_EDGE('',*,*,#2096,.F.);
#2786=ORIENTED_EDGE('',*,*,#2098,.F.);
#2787=ORIENTED_EDGE('',*,*,#2099,.T.);
#2788=ORIENTED_EDGE('',*,*,#2100,.F.);
#2789=ORIENTED_EDGE('',*,*,#2099,.F.);
#2790=ORIENTED_EDGE('',*,*,#2101,.F.);
#2791=ORIENTED_EDGE('',*,*,#2102,.T.);
#2792=ORIENTED_EDGE('',*,*,#2103,.T.);
#2793=ORIENTED_EDGE('',*,*,#2102,.F.);
#2794=ORIENTED_EDGE('',*,*,#2104,.F.);
#2795=ORIENTED_EDGE('',*,*,#2101,.T.);
#2796=ORIENTED_EDGE('',*,*,#2105,.F.);
#2797=ORIENTED_EDGE('',*,*,#2106,.T.);
#2798=ORIENTED_EDGE('',*,*,#2104,.T.);
#2799=ORIENTED_EDGE('',*,*,#2106,.F.);
#2800=ORIENTED_EDGE('',*,*,#2107,.F.);
#2801=ORIENTED_EDGE('',*,*,#2108,.T.);
#2802=ORIENTED_EDGE('',*,*,#2109,.T.);
#2803=ORIENTED_EDGE('',*,*,#2108,.F.);
#2804=ORIENTED_EDGE('',*,*,#2107,.T.);
#2805=ORIENTED_EDGE('',*,*,#2105,.T.);
#2806=ORIENTED_EDGE('',*,*,#2100,.T.);
#2807=ORIENTED_EDGE('',*,*,#2097,.T.);
#2808=ORIENTED_EDGE('',*,*,#2094,.T.);
#2809=ORIENTED_EDGE('',*,*,#2091,.T.);
#2810=ORIENTED_EDGE('',*,*,#2109,.F.);
#2811=ORIENTED_EDGE('',*,*,#2103,.F.);
#2812=ORIENTED_EDGE('',*,*,#2098,.T.);
#2813=ORIENTED_EDGE('',*,*,#2095,.T.);
#2814=ORIENTED_EDGE('',*,*,#2092,.T.);
#2815=ORIENTED_EDGE('',*,*,#2089,.T.);
#2816=ORIENTED_EDGE('',*,*,#2110,.F.);
#2817=ORIENTED_EDGE('',*,*,#2111,.T.);
#2818=ORIENTED_EDGE('',*,*,#2112,.T.);
#2819=ORIENTED_EDGE('',*,*,#2111,.F.);
#2820=ORIENTED_EDGE('',*,*,#2113,.F.);
#2821=ORIENTED_EDGE('',*,*,#2114,.T.);
#2822=ORIENTED_EDGE('',*,*,#2115,.T.);
#2823=ORIENTED_EDGE('',*,*,#2114,.F.);
#2824=ORIENTED_EDGE('',*,*,#2113,.T.);
#2825=ORIENTED_EDGE('',*,*,#2110,.T.);
#2826=ORIENTED_EDGE('',*,*,#2115,.F.);
#2827=ORIENTED_EDGE('',*,*,#2112,.F.);
#2828=ORIENTED_EDGE('',*,*,#2116,.F.);
#2829=ORIENTED_EDGE('',*,*,#2117,.T.);
#2830=ORIENTED_EDGE('',*,*,#2118,.F.);
#2831=ORIENTED_EDGE('',*,*,#2117,.F.);
#2832=ORIENTED_EDGE('',*,*,#2119,.F.);
#2833=ORIENTED_EDGE('',*,*,#2120,.T.);
#2834=ORIENTED_EDGE('',*,*,#2121,.F.);
#2835=ORIENTED_EDGE('',*,*,#2120,.F.);
#2836=ORIENTED_EDGE('',*,*,#2122,.F.);
#2837=ORIENTED_EDGE('',*,*,#2123,.T.);
#2838=ORIENTED_EDGE('',*,*,#2124,.F.);
#2839=ORIENTED_EDGE('',*,*,#2123,.F.);
#2840=ORIENTED_EDGE('',*,*,#2125,.F.);
#2841=ORIENTED_EDGE('',*,*,#2126,.T.);
#2842=ORIENTED_EDGE('',*,*,#2127,.F.);
#2843=ORIENTED_EDGE('',*,*,#2126,.F.);
#2844=ORIENTED_EDGE('',*,*,#2128,.F.);
#2845=ORIENTED_EDGE('',*,*,#2129,.T.);
#2846=ORIENTED_EDGE('',*,*,#2130,.T.);
#2847=ORIENTED_EDGE('',*,*,#2129,.F.);
#2848=ORIENTED_EDGE('',*,*,#2131,.F.);
#2849=ORIENTED_EDGE('',*,*,#2132,.T.);
#2850=ORIENTED_EDGE('',*,*,#2133,.T.);
#2851=ORIENTED_EDGE('',*,*,#2132,.F.);
#2852=ORIENTED_EDGE('',*,*,#2131,.T.);
#2853=ORIENTED_EDGE('',*,*,#2128,.T.);
#2854=ORIENTED_EDGE('',*,*,#2127,.T.);
#2855=ORIENTED_EDGE('',*,*,#2124,.T.);
#2856=ORIENTED_EDGE('',*,*,#2121,.T.);
#2857=ORIENTED_EDGE('',*,*,#2118,.T.);
#2858=ORIENTED_EDGE('',*,*,#2133,.F.);
#2859=ORIENTED_EDGE('',*,*,#2130,.F.);
#2860=ORIENTED_EDGE('',*,*,#2125,.T.);
#2861=ORIENTED_EDGE('',*,*,#2122,.T.);
#2862=ORIENTED_EDGE('',*,*,#2119,.T.);
#2863=ORIENTED_EDGE('',*,*,#2116,.T.);
#2864=ORIENTED_EDGE('',*,*,#2134,.F.);
#2865=ORIENTED_EDGE('',*,*,#2135,.F.);
#2866=ORIENTED_EDGE('',*,*,#2136,.T.);
#2867=ORIENTED_EDGE('',*,*,#2134,.T.);
#2868=ORIENTED_EDGE('',*,*,#2136,.F.);
#2869=ORIENTED_EDGE('',*,*,#2137,.F.);
#2870=ORIENTED_EDGE('',*,*,#2138,.T.);
#2871=ORIENTED_EDGE('',*,*,#2135,.T.);
#2872=ORIENTED_EDGE('',*,*,#2138,.F.);
#2873=ORIENTED_EDGE('',*,*,#2139,.F.);
#2874=ORIENTED_EDGE('',*,*,#2140,.T.);
#2875=ORIENTED_EDGE('',*,*,#2137,.T.);
#2876=ORIENTED_EDGE('',*,*,#2140,.F.);
#2877=ORIENTED_EDGE('',*,*,#2139,.T.);
#2878=ORIENTED_EDGE('',*,*,#2141,.F.);
#2879=ORIENTED_EDGE('',*,*,#2142,.F.);
#2880=ORIENTED_EDGE('',*,*,#2143,.T.);
#2881=ORIENTED_EDGE('',*,*,#2141,.T.);
#2882=ORIENTED_EDGE('',*,*,#2143,.F.);
#2883=ORIENTED_EDGE('',*,*,#2144,.F.);
#2884=ORIENTED_EDGE('',*,*,#2145,.T.);
#2885=ORIENTED_EDGE('',*,*,#2142,.T.);
#2886=ORIENTED_EDGE('',*,*,#2145,.F.);
#2887=ORIENTED_EDGE('',*,*,#2146,.F.);
#2888=ORIENTED_EDGE('',*,*,#2147,.T.);
#2889=ORIENTED_EDGE('',*,*,#2144,.T.);
#2890=ORIENTED_EDGE('',*,*,#2147,.F.);
#2891=ORIENTED_EDGE('',*,*,#2146,.T.);
#2892=ORIENTED_EDGE('',*,*,#2148,.T.);
#2893=ORIENTED_EDGE('',*,*,#2149,.T.);
#2894=ORIENTED_EDGE('',*,*,#2150,.T.);
#2895=ORIENTED_EDGE('',*,*,#2151,.F.);
#2896=ORIENTED_EDGE('',*,*,#2152,.T.);
#2897=ORIENTED_EDGE('',*,*,#2153,.T.);
#2898=ORIENTED_EDGE('',*,*,#2154,.T.);
#2899=ORIENTED_EDGE('',*,*,#2149,.F.);
#2900=ORIENTED_EDGE('',*,*,#2155,.T.);
#2901=ORIENTED_EDGE('',*,*,#2156,.T.);
#2902=ORIENTED_EDGE('',*,*,#2157,.T.);
#2903=ORIENTED_EDGE('',*,*,#2153,.F.);
#2904=ORIENTED_EDGE('',*,*,#2158,.T.);
#2905=ORIENTED_EDGE('',*,*,#2159,.T.);
#2906=ORIENTED_EDGE('',*,*,#2160,.T.);
#2907=ORIENTED_EDGE('',*,*,#2156,.F.);
#2908=ORIENTED_EDGE('',*,*,#2161,.T.);
#2909=ORIENTED_EDGE('',*,*,#2162,.T.);
#2910=ORIENTED_EDGE('',*,*,#2163,.T.);
#2911=ORIENTED_EDGE('',*,*,#2159,.F.);
#2912=ORIENTED_EDGE('',*,*,#2164,.T.);
#2913=ORIENTED_EDGE('',*,*,#2151,.T.);
#2914=ORIENTED_EDGE('',*,*,#2165,.T.);
#2915=ORIENTED_EDGE('',*,*,#2162,.F.);
#2916=ORIENTED_EDGE('',*,*,#2164,.F.);
#2917=ORIENTED_EDGE('',*,*,#2161,.F.);
#2918=ORIENTED_EDGE('',*,*,#2158,.F.);
#2919=ORIENTED_EDGE('',*,*,#2155,.F.);
#2920=ORIENTED_EDGE('',*,*,#2152,.F.);
#2921=ORIENTED_EDGE('',*,*,#2148,.F.);
#2922=ORIENTED_EDGE('',*,*,#2165,.F.);
#2923=ORIENTED_EDGE('',*,*,#2150,.F.);
#2924=ORIENTED_EDGE('',*,*,#2154,.F.);
#2925=ORIENTED_EDGE('',*,*,#2157,.F.);
#2926=ORIENTED_EDGE('',*,*,#2160,.F.);
#2927=ORIENTED_EDGE('',*,*,#2163,.F.);
#2928=CYLINDRICAL_SURFACE('',#3448,0.33);
#2929=CYLINDRICAL_SURFACE('',#3451,0.33);
#2930=CYLINDRICAL_SURFACE('',#3454,0.505);
#2931=CYLINDRICAL_SURFACE('',#3469,0.33);
#2932=CYLINDRICAL_SURFACE('',#3472,0.33);
#2933=CYLINDRICAL_SURFACE('',#3475,0.505);
#2934=CYLINDRICAL_SURFACE('',#3490,0.165);
#2935=CYLINDRICAL_SURFACE('',#3494,0.165);
#2936=CYLINDRICAL_SURFACE('',#3504,0.6);
#2937=CYLINDRICAL_SURFACE('',#3505,0.5);
#2938=CYLINDRICAL_SURFACE('',#3507,0.5);
#2939=CYLINDRICAL_SURFACE('',#3512,0.505);
#2940=CYLINDRICAL_SURFACE('',#3515,0.8);
#2941=CYLINDRICAL_SURFACE('',#3521,0.505);
#2942=CYLINDRICAL_SURFACE('',#3524,0.8);
#2943=CYLINDRICAL_SURFACE('',#3530,0.25);
#2944=CYLINDRICAL_SURFACE('',#3533,0.25);
#2945=CYLINDRICAL_SURFACE('',#3536,0.25);
#2946=CYLINDRICAL_SURFACE('',#3539,0.25);
#2947=CYLINDRICAL_SURFACE('',#3556,0.32);
#2948=CYLINDRICAL_SURFACE('',#3559,0.6);
#2949=CYLINDRICAL_SURFACE('',#3579,0.5);
#2950=CYLINDRICAL_SURFACE('',#3587,0.2942);
#2951=CYLINDRICAL_SURFACE('',#3589,0.225);
#2952=CYLINDRICAL_SURFACE('',#3592,1.1);
#2953=CYLINDRICAL_SURFACE('',#3598,0.605);
#2954=CYLINDRICAL_SURFACE('',#3601,1.);
#2955=CYLINDRICAL_SURFACE('',#3614,0.976185);
#2956=CYLINDRICAL_SURFACE('',#3616,0.5);
#2957=CYLINDRICAL_SURFACE('',#3622,0.976185);
#2958=CYLINDRICAL_SURFACE('',#3634,1.023815);
#2959=CYLINDRICAL_SURFACE('',#3641,1.5);
#2960=CYLINDRICAL_SURFACE('',#3646,1.023815);
#2961=CYLINDRICAL_SURFACE('',#3668,1.019052);
#2962=CYLINDRICAL_SURFACE('',#3708,0.980948);
#2963=CYLINDRICAL_SURFACE('',#3722,1.013815);
#2964=CYLINDRICAL_SURFACE('',#3726,0.991185);
#2965=CYLINDRICAL_SURFACE('',#3730,1.013815);
#2966=CYLINDRICAL_SURFACE('',#3734,0.991185);
#2967=CYLINDRICAL_SURFACE('',#3742,0.165);
#2968=CYLINDRICAL_SURFACE('',#3745,0.165);
#2969=CYLINDRICAL_SURFACE('',#3748,0.165);
#2970=CYLINDRICAL_SURFACE('',#3751,0.165);
#2971=CYLINDRICAL_SURFACE('',#3754,1.2);
#2972=CYLINDRICAL_SURFACE('',#3759,1.5);
#2973=CYLINDRICAL_SURFACE('',#3761,2.2);
#2974=CYLINDRICAL_SURFACE('',#3767,0.165);
#2975=CYLINDRICAL_SURFACE('',#3770,0.165);
#2976=CYLINDRICAL_SURFACE('',#3773,0.165);
#2977=CYLINDRICAL_SURFACE('',#3776,0.165);
#2978=CYLINDRICAL_SURFACE('',#3779,1.2);
#2979=CYLINDRICAL_SURFACE('',#3784,1.5);
#2980=CYLINDRICAL_SURFACE('',#3786,2.2);
#2981=CYLINDRICAL_SURFACE('',#3792,2.2);
#2982=CYLINDRICAL_SURFACE('',#3795,2.5);
#2983=CYLINDRICAL_SURFACE('',#3801,0.225);
#2984=CYLINDRICAL_SURFACE('',#3804,0.225);
#2985=CYLINDRICAL_SURFACE('',#3807,0.225);
#2986=CYLINDRICAL_SURFACE('',#3810,0.225);
#2987=CYLINDRICAL_SURFACE('',#3813,1.2);
#2988=CYLINDRICAL_SURFACE('',#3816,2.5);
#2989=CYLINDRICAL_SURFACE('',#3826,0.35);
#2990=CYLINDRICAL_SURFACE('',#3834,0.1954);
#2991=ADVANCED_FACE('',(#516),#2928,.F.);
#2992=ADVANCED_FACE('',(#517),#2929,.F.);
#2993=ADVANCED_FACE('',(#518),#2930,.F.);
#2994=ADVANCED_FACE('',(#519,#336,#337,#338),#417,.T.);
#2995=ADVANCED_FACE('',(#520),#418,.T.);
#2996=ADVANCED_FACE('',(#521),#419,.T.);
#2997=ADVANCED_FACE('',(#522),#420,.T.);
#2998=ADVANCED_FACE('',(#523),#421,.F.);
#2999=ADVANCED_FACE('',(#524,#339),#422,.T.);
#3000=ADVANCED_FACE('',(#525),#423,.T.);
#3001=ADVANCED_FACE('',(#526,#340),#424,.T.);
#3002=ADVANCED_FACE('',(#527),#425,.T.);
#3003=ADVANCED_FACE('',(#528),#426,.T.);
#3004=ADVANCED_FACE('',(#529,#341,#342),#427,.F.);
#3005=ADVANCED_FACE('',(#530),#2931,.F.);
#3006=ADVANCED_FACE('',(#531),#2932,.F.);
#3007=ADVANCED_FACE('',(#532),#2933,.F.);
#3008=ADVANCED_FACE('',(#533,#343,#344,#345),#428,.T.);
#3009=ADVANCED_FACE('',(#534),#429,.T.);
#3010=ADVANCED_FACE('',(#535),#430,.T.);
#3011=ADVANCED_FACE('',(#536),#431,.T.);
#3012=ADVANCED_FACE('',(#537),#432,.F.);
#3013=ADVANCED_FACE('',(#538,#346),#433,.T.);
#3014=ADVANCED_FACE('',(#539),#434,.T.);
#3015=ADVANCED_FACE('',(#540,#347),#435,.T.);
#3016=ADVANCED_FACE('',(#541),#436,.T.);
#3017=ADVANCED_FACE('',(#542),#437,.T.);
#3018=ADVANCED_FACE('',(#543,#348,#349),#438,.F.);
#3019=ADVANCED_FACE('',(#544),#2934,.F.);
#3020=ADVANCED_FACE('',(#545),#439,.T.);
#3021=ADVANCED_FACE('',(#546),#2935,.F.);
#3022=ADVANCED_FACE('',(#547),#440,.F.);
#3023=ADVANCED_FACE('',(#548,#350),#441,.T.);
#3024=ADVANCED_FACE('',(#549,#351),#442,.F.);
#3025=ADVANCED_FACE('',(#550),#2936,.T.);
#3026=ADVANCED_FACE('',(#551),#2937,.T.);
#3027=ADVANCED_FACE('',(#552),#2938,.T.);
#3028=ADVANCED_FACE('',(#553,#352),#443,.T.);
#3029=ADVANCED_FACE('',(#554,#353),#444,.F.);
#3030=ADVANCED_FACE('',(#555),#2939,.F.);
#3031=ADVANCED_FACE('',(#556),#2940,.T.);
#3032=ADVANCED_FACE('',(#557,#354),#445,.T.);
#3033=ADVANCED_FACE('',(#558,#355),#446,.F.);
#3034=ADVANCED_FACE('',(#559),#2941,.F.);
#3035=ADVANCED_FACE('',(#560),#2942,.T.);
#3036=ADVANCED_FACE('',(#561,#356),#447,.T.);
#3037=ADVANCED_FACE('',(#562,#357),#448,.F.);
#3038=ADVANCED_FACE('',(#563),#2943,.F.);
#3039=ADVANCED_FACE('',(#564),#2944,.F.);
#3040=ADVANCED_FACE('',(#565),#2945,.F.);
#3041=ADVANCED_FACE('',(#566),#2946,.F.);
#3042=ADVANCED_FACE('',(#567),#449,.T.);
#3043=ADVANCED_FACE('',(#568),#450,.T.);
#3044=ADVANCED_FACE('',(#569),#451,.T.);
#3045=ADVANCED_FACE('',(#570),#452,.T.);
#3046=ADVANCED_FACE('',(#571,#358,#359,#360,#361),#453,.T.);
#3047=ADVANCED_FACE('',(#572,#362,#363,#364,#365),#454,.F.);
#3048=ADVANCED_FACE('',(#573),#455,.T.);
#3049=ADVANCED_FACE('',(#574),#456,.T.);
#3050=ADVANCED_FACE('',(#575),#457,.T.);
#3051=ADVANCED_FACE('',(#576),#458,.T.);
#3052=ADVANCED_FACE('',(#577),#459,.T.);
#3053=ADVANCED_FACE('',(#578),#460,.F.);
#3054=ADVANCED_FACE('',(#579),#2947,.F.);
#3055=ADVANCED_FACE('',(#580),#2948,.T.);
#3056=ADVANCED_FACE('',(#581,#366),#461,.T.);
#3057=ADVANCED_FACE('',(#582,#367),#462,.F.);
#3058=ADVANCED_FACE('',(#583),#463,.F.);
#3059=ADVANCED_FACE('',(#584),#464,.F.);
#3060=ADVANCED_FACE('',(#585),#465,.F.);
#3061=ADVANCED_FACE('',(#586),#466,.F.);
#3062=ADVANCED_FACE('',(#587),#467,.F.);
#3063=ADVANCED_FACE('',(#588),#468,.F.);
#3064=ADVANCED_FACE('',(#589),#469,.F.);
#3065=ADVANCED_FACE('',(#590),#470,.F.);
#3066=ADVANCED_FACE('',(#591),#471,.F.);
#3067=ADVANCED_FACE('',(#592),#472,.T.);
#3068=ADVANCED_FACE('',(#593),#223,.T.);
#3069=ADVANCED_FACE('',(#594),#2949,.T.);
#3070=ADVANCED_FACE('',(#595),#224,.T.);
#3071=ADVANCED_FACE('',(#596,#368),#473,.T.);
#3072=ADVANCED_FACE('',(#597),#225,.T.);
#3073=ADVANCED_FACE('',(#598),#2950,.T.);
#3074=ADVANCED_FACE('',(#599),#2951,.F.);
#3075=ADVANCED_FACE('',(#600),#2952,.T.);
#3076=ADVANCED_FACE('',(#601,#369),#474,.T.);
#3077=ADVANCED_FACE('',(#602,#370),#475,.F.);
#3078=ADVANCED_FACE('',(#603),#2953,.F.);
#3079=ADVANCED_FACE('',(#604),#2954,.T.);
#3080=ADVANCED_FACE('',(#605,#371),#476,.T.);
#3081=ADVANCED_FACE('',(#606,#372),#477,.F.);
#3082=ADVANCED_FACE('',(#607),#221,.F.);
#3083=ADVANCED_FACE('',(#608),#2955,.T.);
#3084=ADVANCED_FACE('',(#609),#2956,.F.);
#3085=ADVANCED_FACE('',(#610),#226,.F.);
#3086=ADVANCED_FACE('',(#611,#373),#478,.T.);
#3087=ADVANCED_FACE('',(#612),#2957,.T.);
#3088=ADVANCED_FACE('',(#613,#374),#479,.T.);
#3089=ADVANCED_FACE('',(#614),#227,.F.);
#3090=ADVANCED_FACE('',(#615),#222,.F.);
#3091=ADVANCED_FACE('',(#616),#2958,.F.);
#3092=ADVANCED_FACE('',(#617,#375),#480,.T.);
#3093=ADVANCED_FACE('',(#618),#228,.T.);
#3094=ADVANCED_FACE('',(#619),#2959,.T.);
#3095=ADVANCED_FACE('',(#620),#229,.T.);
#3096=ADVANCED_FACE('',(#621,#376),#481,.T.);
#3097=ADVANCED_FACE('',(#622),#2960,.F.);
#3098=ADVANCED_FACE('',(#623),#205,.T.);
#3099=ADVANCED_FACE('',(#624),#206,.T.);
#3100=ADVANCED_FACE('',(#625),#207,.T.);
#3101=ADVANCED_FACE('',(#626),#208,.T.);
#3102=ADVANCED_FACE('',(#627),#209,.T.);
#3103=ADVANCED_FACE('',(#628),#210,.T.);
#3104=ADVANCED_FACE('',(#629),#211,.T.);
#3105=ADVANCED_FACE('',(#630),#212,.T.);
#3106=ADVANCED_FACE('',(#631),#213,.F.);
#3107=ADVANCED_FACE('',(#632),#2961,.T.);
#3108=ADVANCED_FACE('',(#633),#482,.T.);
#3109=ADVANCED_FACE('',(#634),#214,.F.);
#3110=ADVANCED_FACE('',(#635),#483,.T.);
#3111=ADVANCED_FACE('',(#636),#215,.F.);
#3112=ADVANCED_FACE('',(#637),#484,.T.);
#3113=ADVANCED_FACE('',(#638),#216,.F.);
#3114=ADVANCED_FACE('',(#639),#485,.T.);
#3115=ADVANCED_FACE('',(#640),#217,.F.);
#3116=ADVANCED_FACE('',(#641),#486,.T.);
#3117=ADVANCED_FACE('',(#642),#218,.F.);
#3118=ADVANCED_FACE('',(#643),#487,.T.);
#3119=ADVANCED_FACE('',(#644),#219,.F.);
#3120=ADVANCED_FACE('',(#645),#2962,.F.);
#3121=ADVANCED_FACE('',(#646),#488,.T.);
#3122=ADVANCED_FACE('',(#647),#220,.F.);
#3123=ADVANCED_FACE('',(#648,#377),#489,.T.);
#3124=ADVANCED_FACE('',(#649),#490,.T.);
#3125=ADVANCED_FACE('',(#650,#378),#491,.T.);
#3126=ADVANCED_FACE('',(#651),#2963,.T.);
#3127=ADVANCED_FACE('',(#652,#379),#492,.T.);
#3128=ADVANCED_FACE('',(#653),#2964,.F.);
#3129=ADVANCED_FACE('',(#654,#380),#493,.T.);
#3130=ADVANCED_FACE('',(#655),#2965,.T.);
#3131=ADVANCED_FACE('',(#656,#381),#494,.T.);
#3132=ADVANCED_FACE('',(#657),#2966,.F.);
#3133=ADVANCED_FACE('',(#658),#2967,.F.);
#3134=ADVANCED_FACE('',(#659),#2968,.F.);
#3135=ADVANCED_FACE('',(#660),#2969,.F.);
#3136=ADVANCED_FACE('',(#661),#2970,.F.);
#3137=ADVANCED_FACE('',(#662),#2971,.F.);
#3138=ADVANCED_FACE('',(#663,#382),#495,.F.);
#3139=ADVANCED_FACE('',(#664),#2972,.F.);
#3140=ADVANCED_FACE('',(#665),#2973,.T.);
#3141=ADVANCED_FACE('',(#666,#383,#384,#385,#386,#387),#496,.T.);
#3142=ADVANCED_FACE('',(#667,#388,#389,#390,#391,#392),#497,.F.);
#3143=ADVANCED_FACE('',(#668),#2974,.F.);
#3144=ADVANCED_FACE('',(#669),#2975,.F.);
#3145=ADVANCED_FACE('',(#670),#2976,.F.);
#3146=ADVANCED_FACE('',(#671),#2977,.F.);
#3147=ADVANCED_FACE('',(#672),#2978,.F.);
#3148=ADVANCED_FACE('',(#673,#393),#498,.T.);
#3149=ADVANCED_FACE('',(#674),#2979,.F.);
#3150=ADVANCED_FACE('',(#675),#2980,.T.);
#3151=ADVANCED_FACE('',(#676,#394,#395,#396,#397,#398),#499,.T.);
#3152=ADVANCED_FACE('',(#677,#399,#400,#401,#402,#403),#500,.F.);
#3153=ADVANCED_FACE('',(#678),#2981,.F.);
#3154=ADVANCED_FACE('',(#679),#2982,.T.);
#3155=ADVANCED_FACE('',(#680,#404),#501,.T.);
#3156=ADVANCED_FACE('',(#681,#405),#502,.F.);
#3157=ADVANCED_FACE('',(#682),#2983,.F.);
#3158=ADVANCED_FACE('',(#683),#2984,.F.);
#3159=ADVANCED_FACE('',(#684),#2985,.F.);
#3160=ADVANCED_FACE('',(#685),#2986,.F.);
#3161=ADVANCED_FACE('',(#686),#2987,.F.);
#3162=ADVANCED_FACE('',(#687),#2988,.T.);
#3163=ADVANCED_FACE('',(#688,#406,#407,#408,#409,#410),#503,.T.);
#3164=ADVANCED_FACE('',(#689,#411,#412,#413,#414,#415),#504,.F.);
#3165=ADVANCED_FACE('',(#690),#505,.T.);
#3166=ADVANCED_FACE('',(#691),#230,.T.);
#3167=ADVANCED_FACE('',(#692),#2989,.T.);
#3168=ADVANCED_FACE('',(#693),#231,.T.);
#3169=ADVANCED_FACE('',(#694,#416),#506,.T.);
#3170=ADVANCED_FACE('',(#695),#232,.T.);
#3171=ADVANCED_FACE('',(#696),#2990,.T.);
#3172=ADVANCED_FACE('',(#697),#233,.T.);
#3173=ADVANCED_FACE('',(#698),#507,.T.);
#3174=ADVANCED_FACE('',(#699),#508,.F.);
#3175=ADVANCED_FACE('',(#700),#509,.F.);
#3176=ADVANCED_FACE('',(#701),#510,.F.);
#3177=ADVANCED_FACE('',(#702),#511,.F.);
#3178=ADVANCED_FACE('',(#703),#512,.F.);
#3179=ADVANCED_FACE('',(#704),#513,.F.);
#3180=ADVANCED_FACE('',(#705),#514,.F.);
#3181=ADVANCED_FACE('',(#706),#515,.F.);
#3182=CLOSED_SHELL('',(#2991,#2992,#2993,#2994,#2995,#2996,#2997,#2998,
#2999,#3000,#3001,#3002,#3003,#3004));
#3183=CLOSED_SHELL('',(#3005,#3006,#3007,#3008,#3009,#3010,#3011,#3012,
#3013,#3014,#3015,#3016,#3017,#3018));
#3184=CLOSED_SHELL('',(#3019,#3020,#3021,#3022,#3023,#3024,#3025,#3026,
#3027,#3028,#3029));
#3185=CLOSED_SHELL('',(#3030,#3031,#3032,#3033));
#3186=CLOSED_SHELL('',(#3034,#3035,#3036,#3037));
#3187=CLOSED_SHELL('',(#3038,#3039,#3040,#3041,#3042,#3043,#3044,#3045,
#3046,#3047));
#3188=CLOSED_SHELL('',(#3048,#3049,#3050,#3051,#3052,#3053));
#3189=CLOSED_SHELL('',(#3054,#3055,#3056,#3057));
#3190=CLOSED_SHELL('',(#3058,#3059,#3060,#3061,#3062,#3063,#3064,#3065));
#3191=CLOSED_SHELL('',(#3066,#3067,#3068,#3069,#3070,#3071,#3072,#3073));
#3192=CLOSED_SHELL('',(#3074,#3075,#3076,#3077));
#3193=CLOSED_SHELL('',(#3078,#3079,#3080,#3081));
#3194=CLOSED_SHELL('',(#3082,#3083,#3084,#3085,#3086,#3087,#3088,#3089));
#3195=CLOSED_SHELL('',(#3090,#3091,#3092,#3093,#3094,#3095,#3096,#3097));
#3196=CLOSED_SHELL('',(#3098));
#3197=CLOSED_SHELL('',(#3099));
#3198=CLOSED_SHELL('',(#3100));
#3199=CLOSED_SHELL('',(#3101));
#3200=CLOSED_SHELL('',(#3102));
#3201=CLOSED_SHELL('',(#3103));
#3202=CLOSED_SHELL('',(#3104));
#3203=CLOSED_SHELL('',(#3105));
#3204=CLOSED_SHELL('',(#3106,#3107,#3108,#3109,#3110,#3111,#3112,#3113,
#3114,#3115,#3116,#3117,#3118,#3119,#3120,#3121,#3122,#3123,#3124));
#3205=CLOSED_SHELL('',(#3125,#3126,#3127,#3128));
#3206=CLOSED_SHELL('',(#3129,#3130,#3131,#3132));
#3207=CLOSED_SHELL('',(#3133,#3134,#3135,#3136,#3137,#3138,#3139,#3140,
#3141,#3142));
#3208=CLOSED_SHELL('',(#3143,#3144,#3145,#3146,#3147,#3148,#3149,#3150,
#3151,#3152));
#3209=CLOSED_SHELL('',(#3153,#3154,#3155,#3156));
#3210=CLOSED_SHELL('',(#3157,#3158,#3159,#3160,#3161,#3162,#3163,#3164));
#3211=CLOSED_SHELL('',(#3165,#3166,#3167,#3168,#3169,#3170,#3171,#3172,
#3173));
#3212=CLOSED_SHELL('',(#3174,#3175,#3176,#3177,#3178,#3179,#3180,#3181));
#3213=DERIVED_UNIT_ELEMENT(#3255,1.);
#3214=DERIVED_UNIT_ELEMENT(#6243,-3.);
#3215=DERIVED_UNIT_ELEMENT(#3255,1.);
#3216=DERIVED_UNIT_ELEMENT(#6243,-3.);
#3217=DERIVED_UNIT_ELEMENT(#3255,1.);
#3218=DERIVED_UNIT_ELEMENT(#6243,-3.);
#3219=DERIVED_UNIT_ELEMENT(#3255,1.);
#3220=DERIVED_UNIT_ELEMENT(#6243,-3.);
#3221=DERIVED_UNIT_ELEMENT(#3255,1.);
#3222=DERIVED_UNIT_ELEMENT(#6243,-3.);
#3223=DERIVED_UNIT_ELEMENT(#3255,1.);
#3224=DERIVED_UNIT_ELEMENT(#6243,-3.);
#3225=DERIVED_UNIT_ELEMENT(#3255,1.);
#3226=DERIVED_UNIT_ELEMENT(#6243,-3.);
#3227=DERIVED_UNIT_ELEMENT(#3255,1.);
#3228=DERIVED_UNIT_ELEMENT(#6243,-3.);
#3229=DERIVED_UNIT_ELEMENT(#3255,1.);
#3230=DERIVED_UNIT_ELEMENT(#6243,-3.);
#3231=DERIVED_UNIT_ELEMENT(#3255,1.);
#3232=DERIVED_UNIT_ELEMENT(#6243,-3.);
#3233=DERIVED_UNIT_ELEMENT(#3255,1.);
#3234=DERIVED_UNIT_ELEMENT(#6243,-3.);
#3235=DERIVED_UNIT_ELEMENT(#3255,1.);
#3236=DERIVED_UNIT_ELEMENT(#6243,-3.);
#3237=DERIVED_UNIT_ELEMENT(#3255,1.);
#3238=DERIVED_UNIT_ELEMENT(#6243,-3.);
#3239=DERIVED_UNIT_ELEMENT(#3255,1.);
#3240=DERIVED_UNIT_ELEMENT(#6243,-3.);
#3241=DERIVED_UNIT_ELEMENT(#3255,1.);
#3242=DERIVED_UNIT_ELEMENT(#6243,-3.);
#3243=DERIVED_UNIT_ELEMENT(#3255,1.);
#3244=DERIVED_UNIT_ELEMENT(#6243,-3.);
#3245=DERIVED_UNIT_ELEMENT(#3255,1.);
#3246=DERIVED_UNIT_ELEMENT(#6243,-3.);
#3247=DERIVED_UNIT_ELEMENT(#3255,1.);
#3248=DERIVED_UNIT_ELEMENT(#6243,-3.);
#3249=DERIVED_UNIT_ELEMENT(#3255,1.);
#3250=DERIVED_UNIT_ELEMENT(#6243,-3.);
#3251=DERIVED_UNIT_ELEMENT(#3255,1.);
#3252=DERIVED_UNIT_ELEMENT(#6243,-3.);
#3253=DERIVED_UNIT_ELEMENT(#3255,1.);
#3254=DERIVED_UNIT_ELEMENT(#6243,-3.);
#3255=(
MASS_UNIT()
NAMED_UNIT(*)
SI_UNIT(.KILO.,.GRAM.)
);
#3256=DERIVED_UNIT((#3213,#3214));
#3257=DERIVED_UNIT((#3215,#3216));
#3258=DERIVED_UNIT((#3217,#3218));
#3259=DERIVED_UNIT((#3219,#3220));
#3260=DERIVED_UNIT((#3221,#3222));
#3261=DERIVED_UNIT((#3223,#3224));
#3262=DERIVED_UNIT((#3225,#3226));
#3263=DERIVED_UNIT((#3227,#3228));
#3264=DERIVED_UNIT((#3229,#3230));
#3265=DERIVED_UNIT((#3231,#3232));
#3266=DERIVED_UNIT((#3233,#3234));
#3267=DERIVED_UNIT((#3235,#3236));
#3268=DERIVED_UNIT((#3237,#3238));
#3269=DERIVED_UNIT((#3239,#3240));
#3270=DERIVED_UNIT((#3241,#3242));
#3271=DERIVED_UNIT((#3243,#3244));
#3272=DERIVED_UNIT((#3245,#3246));
#3273=DERIVED_UNIT((#3247,#3248));
#3274=DERIVED_UNIT((#3249,#3250));
#3275=DERIVED_UNIT((#3251,#3252));
#3276=DERIVED_UNIT((#3253,#3254));
#3277=MEASURE_REPRESENTATION_ITEM('density measure',
POSITIVE_RATIO_MEASURE(7850.),#3256);
#3278=MEASURE_REPRESENTATION_ITEM('density measure',
POSITIVE_RATIO_MEASURE(7850.),#3257);
#3279=MEASURE_REPRESENTATION_ITEM('density measure',
POSITIVE_RATIO_MEASURE(7850.),#3258);
#3280=MEASURE_REPRESENTATION_ITEM('density measure',
POSITIVE_RATIO_MEASURE(7850.),#3259);
#3281=MEASURE_REPRESENTATION_ITEM('density measure',
POSITIVE_RATIO_MEASURE(7850.),#3260);
#3282=MEASURE_REPRESENTATION_ITEM('density measure',
POSITIVE_RATIO_MEASURE(7850.),#3261);
#3283=MEASURE_REPRESENTATION_ITEM('density measure',
POSITIVE_RATIO_MEASURE(7850.),#3262);
#3284=MEASURE_REPRESENTATION_ITEM('density measure',
POSITIVE_RATIO_MEASURE(7850.),#3263);
#3285=MEASURE_REPRESENTATION_ITEM('density measure',
POSITIVE_RATIO_MEASURE(7850.),#3264);
#3286=MEASURE_REPRESENTATION_ITEM('density measure',
POSITIVE_RATIO_MEASURE(7850.),#3265);
#3287=MEASURE_REPRESENTATION_ITEM('density measure',
POSITIVE_RATIO_MEASURE(7850.),#3266);
#3288=MEASURE_REPRESENTATION_ITEM('density measure',
POSITIVE_RATIO_MEASURE(7850.),#3267);
#3289=MEASURE_REPRESENTATION_ITEM('density measure',
POSITIVE_RATIO_MEASURE(7850.),#3268);
#3290=MEASURE_REPRESENTATION_ITEM('density measure',
POSITIVE_RATIO_MEASURE(7850.),#3269);
#3291=MEASURE_REPRESENTATION_ITEM('density measure',
POSITIVE_RATIO_MEASURE(7850.),#3270);
#3292=MEASURE_REPRESENTATION_ITEM('density measure',
POSITIVE_RATIO_MEASURE(7850.),#3271);
#3293=MEASURE_REPRESENTATION_ITEM('density measure',
POSITIVE_RATIO_MEASURE(7850.),#3272);
#3294=MEASURE_REPRESENTATION_ITEM('density measure',
POSITIVE_RATIO_MEASURE(7850.),#3273);
#3295=MEASURE_REPRESENTATION_ITEM('density measure',
POSITIVE_RATIO_MEASURE(7850.),#3274);
#3296=MEASURE_REPRESENTATION_ITEM('density measure',
POSITIVE_RATIO_MEASURE(7850.),#3275);
#3297=MEASURE_REPRESENTATION_ITEM('density measure',
POSITIVE_RATIO_MEASURE(7850.),#3276);
#3298=PROPERTY_DEFINITION_REPRESENTATION(#3403,#3340);
#3299=PROPERTY_DEFINITION_REPRESENTATION(#3404,#3341);
#3300=PROPERTY_DEFINITION_REPRESENTATION(#3405,#3342);
#3301=PROPERTY_DEFINITION_REPRESENTATION(#3406,#3343);
#3302=PROPERTY_DEFINITION_REPRESENTATION(#3407,#3344);
#3303=PROPERTY_DEFINITION_REPRESENTATION(#3408,#3345);
#3304=PROPERTY_DEFINITION_REPRESENTATION(#3409,#3346);
#3305=PROPERTY_DEFINITION_REPRESENTATION(#3410,#3347);
#3306=PROPERTY_DEFINITION_REPRESENTATION(#3411,#3348);
#3307=PROPERTY_DEFINITION_REPRESENTATION(#3412,#3349);
#3308=PROPERTY_DEFINITION_REPRESENTATION(#3413,#3350);
#3309=PROPERTY_DEFINITION_REPRESENTATION(#3414,#3351);
#3310=PROPERTY_DEFINITION_REPRESENTATION(#3415,#3352);
#3311=PROPERTY_DEFINITION_REPRESENTATION(#3416,#3353);
#3312=PROPERTY_DEFINITION_REPRESENTATION(#3417,#3354);
#3313=PROPERTY_DEFINITION_REPRESENTATION(#3418,#3355);
#3314=PROPERTY_DEFINITION_REPRESENTATION(#3419,#3356);
#3315=PROPERTY_DEFINITION_REPRESENTATION(#3420,#3357);
#3316=PROPERTY_DEFINITION_REPRESENTATION(#3421,#3358);
#3317=PROPERTY_DEFINITION_REPRESENTATION(#3422,#3359);
#3318=PROPERTY_DEFINITION_REPRESENTATION(#3423,#3360);
#3319=PROPERTY_DEFINITION_REPRESENTATION(#3424,#3361);
#3320=PROPERTY_DEFINITION_REPRESENTATION(#3425,#3362);
#3321=PROPERTY_DEFINITION_REPRESENTATION(#3426,#3363);
#3322=PROPERTY_DEFINITION_REPRESENTATION(#3427,#3364);
#3323=PROPERTY_DEFINITION_REPRESENTATION(#3428,#3365);
#3324=PROPERTY_DEFINITION_REPRESENTATION(#3429,#3366);
#3325=PROPERTY_DEFINITION_REPRESENTATION(#3430,#3367);
#3326=PROPERTY_DEFINITION_REPRESENTATION(#3431,#3368);
#3327=PROPERTY_DEFINITION_REPRESENTATION(#3432,#3369);
#3328=PROPERTY_DEFINITION_REPRESENTATION(#3433,#3370);
#3329=PROPERTY_DEFINITION_REPRESENTATION(#3434,#3371);
#3330=PROPERTY_DEFINITION_REPRESENTATION(#3435,#3372);
#3331=PROPERTY_DEFINITION_REPRESENTATION(#3436,#3373);
#3332=PROPERTY_DEFINITION_REPRESENTATION(#3437,#3374);
#3333=PROPERTY_DEFINITION_REPRESENTATION(#3438,#3375);
#3334=PROPERTY_DEFINITION_REPRESENTATION(#3439,#3376);
#3335=PROPERTY_DEFINITION_REPRESENTATION(#3440,#3377);
#3336=PROPERTY_DEFINITION_REPRESENTATION(#3441,#3378);
#3337=PROPERTY_DEFINITION_REPRESENTATION(#3442,#3379);
#3338=PROPERTY_DEFINITION_REPRESENTATION(#3443,#3380);
#3339=PROPERTY_DEFINITION_REPRESENTATION(#3444,#3381);
#3340=REPRESENTATION('material name',(#3382),#6218);
#3341=REPRESENTATION('density',(#3277),#6218);
#3342=REPRESENTATION('material name',(#3383),#6219);
#3343=REPRESENTATION('density',(#3278),#6219);
#3344=REPRESENTATION('material name',(#3384),#6220);
#3345=REPRESENTATION('density',(#3279),#6220);
#3346=REPRESENTATION('material name',(#3385),#6221);
#3347=REPRESENTATION('density',(#3280),#6221);
#3348=REPRESENTATION('material name',(#3386),#6222);
#3349=REPRESENTATION('density',(#3281),#6222);
#3350=REPRESENTATION('material name',(#3387),#6223);
#3351=REPRESENTATION('density',(#3282),#6223);
#3352=REPRESENTATION('material name',(#3388),#6224);
#3353=REPRESENTATION('density',(#3283),#6224);
#3354=REPRESENTATION('material name',(#3389),#6225);
#3355=REPRESENTATION('density',(#3284),#6225);
#3356=REPRESENTATION('material name',(#3390),#6226);
#3357=REPRESENTATION('density',(#3285),#6226);
#3358=REPRESENTATION('material name',(#3391),#6227);
#3359=REPRESENTATION('density',(#3286),#6227);
#3360=REPRESENTATION('material name',(#3392),#6228);
#3361=REPRESENTATION('density',(#3287),#6228);
#3362=REPRESENTATION('material name',(#3393),#6230);
#3363=REPRESENTATION('density',(#3288),#6230);
#3364=REPRESENTATION('material name',(#3394),#6231);
#3365=REPRESENTATION('density',(#3289),#6231);
#3366=REPRESENTATION('material name',(#3395),#6232);
#3367=REPRESENTATION('density',(#3290),#6232);
#3368=REPRESENTATION('material name',(#3396),#6233);
#3369=REPRESENTATION('density',(#3291),#6233);
#3370=REPRESENTATION('material name',(#3397),#6234);
#3371=REPRESENTATION('density',(#3292),#6234);
#3372=REPRESENTATION('material name',(#3398),#6236);
#3373=REPRESENTATION('density',(#3293),#6236);
#3374=REPRESENTATION('material name',(#3399),#6237);
#3375=REPRESENTATION('density',(#3294),#6237);
#3376=REPRESENTATION('material name',(#3400),#6238);
#3377=REPRESENTATION('density',(#3295),#6238);
#3378=REPRESENTATION('material name',(#3401),#6239);
#3379=REPRESENTATION('density',(#3296),#6239);
#3380=REPRESENTATION('material name',(#3402),#6240);
#3381=REPRESENTATION('density',(#3297),#6240);
#3382=DESCRIPTIVE_REPRESENTATION_ITEM('Steel','Steel');
#3383=DESCRIPTIVE_REPRESENTATION_ITEM('Steel','Steel');
#3384=DESCRIPTIVE_REPRESENTATION_ITEM('Steel','Steel');
#3385=DESCRIPTIVE_REPRESENTATION_ITEM('Steel','Steel');
#3386=DESCRIPTIVE_REPRESENTATION_ITEM('Steel','Steel');
#3387=DESCRIPTIVE_REPRESENTATION_ITEM('Steel','Steel');
#3388=DESCRIPTIVE_REPRESENTATION_ITEM('Steel','Steel');
#3389=DESCRIPTIVE_REPRESENTATION_ITEM('Steel','Steel');
#3390=DESCRIPTIVE_REPRESENTATION_ITEM('Steel','Steel');
#3391=DESCRIPTIVE_REPRESENTATION_ITEM('Steel','Steel');
#3392=DESCRIPTIVE_REPRESENTATION_ITEM('Steel','Steel');
#3393=DESCRIPTIVE_REPRESENTATION_ITEM('Steel','Steel');
#3394=DESCRIPTIVE_REPRESENTATION_ITEM('Steel','Steel');
#3395=DESCRIPTIVE_REPRESENTATION_ITEM('Steel','Steel');
#3396=DESCRIPTIVE_REPRESENTATION_ITEM('Steel','Steel');
#3397=DESCRIPTIVE_REPRESENTATION_ITEM('Steel','Steel');
#3398=DESCRIPTIVE_REPRESENTATION_ITEM('Steel','Steel');
#3399=DESCRIPTIVE_REPRESENTATION_ITEM('Steel','Steel');
#3400=DESCRIPTIVE_REPRESENTATION_ITEM('Steel','Steel');
#3401=DESCRIPTIVE_REPRESENTATION_ITEM('Steel','Steel');
#3402=DESCRIPTIVE_REPRESENTATION_ITEM('Steel','Steel');
#3403=PROPERTY_DEFINITION('material property','material name',#6368);
#3404=PROPERTY_DEFINITION('material property','density of part',#6368);
#3405=PROPERTY_DEFINITION('material property','material name',#6369);
#3406=PROPERTY_DEFINITION('material property','density of part',#6369);
#3407=PROPERTY_DEFINITION('material property','material name',#6370);
#3408=PROPERTY_DEFINITION('material property','density of part',#6370);
#3409=PROPERTY_DEFINITION('material property','material name',#6371);
#3410=PROPERTY_DEFINITION('material property','density of part',#6371);
#3411=PROPERTY_DEFINITION('material property','material name',#6372);
#3412=PROPERTY_DEFINITION('material property','density of part',#6372);
#3413=PROPERTY_DEFINITION('material property','material name',#6373);
#3414=PROPERTY_DEFINITION('material property','density of part',#6373);
#3415=PROPERTY_DEFINITION('material property','material name',#6374);
#3416=PROPERTY_DEFINITION('material property','density of part',#6374);
#3417=PROPERTY_DEFINITION('material property','material name',#6375);
#3418=PROPERTY_DEFINITION('material property','density of part',#6375);
#3419=PROPERTY_DEFINITION('material property','material name',#6376);
#3420=PROPERTY_DEFINITION('material property','density of part',#6376);
#3421=PROPERTY_DEFINITION('material property','material name',#6377);
#3422=PROPERTY_DEFINITION('material property','density of part',#6377);
#3423=PROPERTY_DEFINITION('material property','material name',#6378);
#3424=PROPERTY_DEFINITION('material property','density of part',#6378);
#3425=PROPERTY_DEFINITION('material property','material name',#6380);
#3426=PROPERTY_DEFINITION('material property','density of part',#6380);
#3427=PROPERTY_DEFINITION('material property','material name',#6381);
#3428=PROPERTY_DEFINITION('material property','density of part',#6381);
#3429=PROPERTY_DEFINITION('material property','material name',#6382);
#3430=PROPERTY_DEFINITION('material property','density of part',#6382);
#3431=PROPERTY_DEFINITION('material property','material name',#6383);
#3432=PROPERTY_DEFINITION('material property','density of part',#6383);
#3433=PROPERTY_DEFINITION('material property','material name',#6384);
#3434=PROPERTY_DEFINITION('material property','density of part',#6384);
#3435=PROPERTY_DEFINITION('material property','material name',#6386);
#3436=PROPERTY_DEFINITION('material property','density of part',#6386);
#3437=PROPERTY_DEFINITION('material property','material name',#6387);
#3438=PROPERTY_DEFINITION('material property','density of part',#6387);
#3439=PROPERTY_DEFINITION('material property','material name',#6388);
#3440=PROPERTY_DEFINITION('material property','density of part',#6388);
#3441=PROPERTY_DEFINITION('material property','material name',#6389);
#3442=PROPERTY_DEFINITION('material property','density of part',#6389);
#3443=PROPERTY_DEFINITION('material property','material name',#6390);
#3444=PROPERTY_DEFINITION('material property','density of part',#6390);
#3445=AXIS2_PLACEMENT_3D('',#4950,#3886,#3887);
#3446=AXIS2_PLACEMENT_3D('',#4951,#3888,#3889);
#3447=AXIS2_PLACEMENT_3D('',#4952,#3890,#3891);
#3448=AXIS2_PLACEMENT_3D('',#4953,#3892,#3893);
#3449=AXIS2_PLACEMENT_3D('',#4955,#3894,#3895);
#3450=AXIS2_PLACEMENT_3D('',#4958,#3897,#3898);
#3451=AXIS2_PLACEMENT_3D('',#4959,#3899,#3900);
#3452=AXIS2_PLACEMENT_3D('',#4961,#3901,#3902);
#3453=AXIS2_PLACEMENT_3D('',#4964,#3904,#3905);
#3454=AXIS2_PLACEMENT_3D('',#4965,#3906,#3907);
#3455=AXIS2_PLACEMENT_3D('',#4967,#3908,#3909);
#3456=AXIS2_PLACEMENT_3D('',#4970,#3911,#3912);
#3457=AXIS2_PLACEMENT_3D('',#4971,#3913,#3914);
#3458=AXIS2_PLACEMENT_3D('',#4988,#3923,#3924);
#3459=AXIS2_PLACEMENT_3D('',#4994,#3928,#3929);
#3460=AXIS2_PLACEMENT_3D('',#5000,#3933,#3934);
#3461=AXIS2_PLACEMENT_3D('',#5002,#3936,#3937);
#3462=AXIS2_PLACEMENT_3D('',#5004,#3939,#3940);
#3463=AXIS2_PLACEMENT_3D('',#5010,#3944,#3945);
#3464=AXIS2_PLACEMENT_3D('',#5014,#3948,#3949);
#3465=AXIS2_PLACEMENT_3D('',#5018,#3952,#3953);
#3466=AXIS2_PLACEMENT_3D('',#5020,#3955,#3956);
#3467=AXIS2_PLACEMENT_3D('',#5021,#3957,#3958);
#3468=AXIS2_PLACEMENT_3D('',#5022,#3959,#3960);
#3469=AXIS2_PLACEMENT_3D('',#5023,#3961,#3962);
#3470=AXIS2_PLACEMENT_3D('',#5025,#3963,#3964);
#3471=AXIS2_PLACEMENT_3D('',#5028,#3966,#3967);
#3472=AXIS2_PLACEMENT_3D('',#5029,#3968,#3969);
#3473=AXIS2_PLACEMENT_3D('',#5031,#3970,#3971);
#3474=AXIS2_PLACEMENT_3D('',#5034,#3973,#3974);
#3475=AXIS2_PLACEMENT_3D('',#5035,#3975,#3976);
#3476=AXIS2_PLACEMENT_3D('',#5037,#3977,#3978);
#3477=AXIS2_PLACEMENT_3D('',#5040,#3980,#3981);
#3478=AXIS2_PLACEMENT_3D('',#5041,#3982,#3983);
#3479=AXIS2_PLACEMENT_3D('',#5058,#3992,#3993);
#3480=AXIS2_PLACEMENT_3D('',#5064,#3997,#3998);
#3481=AXIS2_PLACEMENT_3D('',#5070,#4002,#4003);
#3482=AXIS2_PLACEMENT_3D('',#5072,#4005,#4006);
#3483=AXIS2_PLACEMENT_3D('',#5074,#4008,#4009);
#3484=AXIS2_PLACEMENT_3D('',#5080,#4013,#4014);
#3485=AXIS2_PLACEMENT_3D('',#5084,#4017,#4018);
#3486=AXIS2_PLACEMENT_3D('',#5088,#4021,#4022);
#3487=AXIS2_PLACEMENT_3D('',#5090,#4024,#4025);
#3488=AXIS2_PLACEMENT_3D('',#5091,#4026,#4027);
#3489=AXIS2_PLACEMENT_3D('',#5092,#4028,#4029);
#3490=AXIS2_PLACEMENT_3D('',#5093,#4030,#4031);
#3491=AXIS2_PLACEMENT_3D('',#5095,#4032,#4033);
#3492=AXIS2_PLACEMENT_3D('',#5098,#4035,#4036);
#3493=AXIS2_PLACEMENT_3D('',#5099,#4037,#4038);
#3494=AXIS2_PLACEMENT_3D('',#5100,#4039,#4040);
#3495=AXIS2_PLACEMENT_3D('',#5102,#4041,#4042);
#3496=AXIS2_PLACEMENT_3D('',#5105,#4044,#4045);
#3497=AXIS2_PLACEMENT_3D('',#5106,#4046,#4047);
#3498=AXIS2_PLACEMENT_3D('',#5107,#4048,#4049);
#3499=AXIS2_PLACEMENT_3D('',#5109,#4050,#4051);
#3500=AXIS2_PLACEMENT_3D('',#5111,#4052,#4053);
#3501=AXIS2_PLACEMENT_3D('',#5112,#4054,#4055);
#3502=AXIS2_PLACEMENT_3D('',#5114,#4056,#4057);
#3503=AXIS2_PLACEMENT_3D('',#5116,#4058,#4059);
#3504=AXIS2_PLACEMENT_3D('',#5117,#4060,#4061);
#3505=AXIS2_PLACEMENT_3D('',#5119,#4063,#4064);
#3506=AXIS2_PLACEMENT_3D('',#5122,#4066,#4067);
#3507=AXIS2_PLACEMENT_3D('',#5123,#4068,#4069);
#3508=AXIS2_PLACEMENT_3D('',#5125,#4070,#4071);
#3509=AXIS2_PLACEMENT_3D('',#5127,#4073,#4074);
#3510=AXIS2_PLACEMENT_3D('',#5128,#4075,#4076);
#3511=AXIS2_PLACEMENT_3D('',#5129,#4077,#4078);
#3512=AXIS2_PLACEMENT_3D('',#5130,#4079,#4080);
#3513=AXIS2_PLACEMENT_3D('',#5132,#4081,#4082);
#3514=AXIS2_PLACEMENT_3D('',#5135,#4084,#4085);
#3515=AXIS2_PLACEMENT_3D('',#5136,#4086,#4087);
#3516=AXIS2_PLACEMENT_3D('',#5138,#4088,#4089);
#3517=AXIS2_PLACEMENT_3D('',#5141,#4091,#4092);
#3518=AXIS2_PLACEMENT_3D('',#5142,#4093,#4094);
#3519=AXIS2_PLACEMENT_3D('',#5143,#4095,#4096);
#3520=AXIS2_PLACEMENT_3D('',#5144,#4097,#4098);
#3521=AXIS2_PLACEMENT_3D('',#5145,#4099,#4100);
#3522=AXIS2_PLACEMENT_3D('',#5147,#4101,#4102);
#3523=AXIS2_PLACEMENT_3D('',#5150,#4104,#4105);
#3524=AXIS2_PLACEMENT_3D('',#5151,#4106,#4107);
#3525=AXIS2_PLACEMENT_3D('',#5153,#4108,#4109);
#3526=AXIS2_PLACEMENT_3D('',#5156,#4111,#4112);
#3527=AXIS2_PLACEMENT_3D('',#5157,#4113,#4114);
#3528=AXIS2_PLACEMENT_3D('',#5158,#4115,#4116);
#3529=AXIS2_PLACEMENT_3D('',#5159,#4117,#4118);
#3530=AXIS2_PLACEMENT_3D('',#5160,#4119,#4120);
#3531=AXIS2_PLACEMENT_3D('',#5162,#4121,#4122);
#3532=AXIS2_PLACEMENT_3D('',#5165,#4124,#4125);
#3533=AXIS2_PLACEMENT_3D('',#5166,#4126,#4127);
#3534=AXIS2_PLACEMENT_3D('',#5168,#4128,#4129);
#3535=AXIS2_PLACEMENT_3D('',#5171,#4131,#4132);
#3536=AXIS2_PLACEMENT_3D('',#5172,#4133,#4134);
#3537=AXIS2_PLACEMENT_3D('',#5174,#4135,#4136);
#3538=AXIS2_PLACEMENT_3D('',#5177,#4138,#4139);
#3539=AXIS2_PLACEMENT_3D('',#5178,#4140,#4141);
#3540=AXIS2_PLACEMENT_3D('',#5180,#4142,#4143);
#3541=AXIS2_PLACEMENT_3D('',#5183,#4145,#4146);
#3542=AXIS2_PLACEMENT_3D('',#5184,#4147,#4148);
#3543=AXIS2_PLACEMENT_3D('',#5193,#4153,#4154);
#3544=AXIS2_PLACEMENT_3D('',#5199,#4158,#4159);
#3545=AXIS2_PLACEMENT_3D('',#5205,#4163,#4164);
#3546=AXIS2_PLACEMENT_3D('',#5208,#4167,#4168);
#3547=AXIS2_PLACEMENT_3D('',#5209,#4169,#4170);
#3548=AXIS2_PLACEMENT_3D('',#5210,#4171,#4172);
#3549=AXIS2_PLACEMENT_3D('',#5211,#4173,#4174);
#3550=AXIS2_PLACEMENT_3D('',#5220,#4179,#4180);
#3551=AXIS2_PLACEMENT_3D('',#5226,#4184,#4185);
#3552=AXIS2_PLACEMENT_3D('',#5232,#4189,#4190);
#3553=AXIS2_PLACEMENT_3D('',#5235,#4193,#4194);
#3554=AXIS2_PLACEMENT_3D('',#5236,#4195,#4196);
#3555=AXIS2_PLACEMENT_3D('',#5237,#4197,#4198);
#3556=AXIS2_PLACEMENT_3D('',#5238,#4199,#4200);
#3557=AXIS2_PLACEMENT_3D('',#5240,#4201,#4202);
#3558=AXIS2_PLACEMENT_3D('',#5243,#4204,#4205);
#3559=AXIS2_PLACEMENT_3D('',#5244,#4206,#4207);
#3560=AXIS2_PLACEMENT_3D('',#5246,#4208,#4209);
#3561=AXIS2_PLACEMENT_3D('',#5249,#4211,#4212);
#3562=AXIS2_PLACEMENT_3D('',#5250,#4213,#4214);
#3563=AXIS2_PLACEMENT_3D('',#5251,#4215,#4216);
#3564=AXIS2_PLACEMENT_3D('',#5252,#4217,#4218);
#3565=AXIS2_PLACEMENT_3D('',#5253,#4219,#4220);
#3566=AXIS2_PLACEMENT_3D('',#5262,#4225,#4226);
#3567=AXIS2_PLACEMENT_3D('',#5268,#4230,#4231);
#3568=AXIS2_PLACEMENT_3D('',#5274,#4235,#4236);
#3569=AXIS2_PLACEMENT_3D('',#5280,#4240,#4241);
#3570=AXIS2_PLACEMENT_3D('',#5286,#4245,#4246);
#3571=AXIS2_PLACEMENT_3D('',#5289,#4249,#4250);
#3572=AXIS2_PLACEMENT_3D('',#5290,#4251,#4252);
#3573=AXIS2_PLACEMENT_3D('',#5291,#4253,#4254);
#3574=AXIS2_PLACEMENT_3D('',#5293,#4255,#4256);
#3575=AXIS2_PLACEMENT_3D('',#5294,#4257,#4258);
#3576=AXIS2_PLACEMENT_3D('',#5296,#4259,#4260);
#3577=AXIS2_PLACEMENT_3D('',#5297,#4261,#4262);
#3578=AXIS2_PLACEMENT_3D('',#5299,#4263,#4264);
#3579=AXIS2_PLACEMENT_3D('',#5301,#4266,#4267);
#3580=AXIS2_PLACEMENT_3D('',#5303,#4268,#4269);
#3581=AXIS2_PLACEMENT_3D('',#5305,#4271,#4272);
#3582=AXIS2_PLACEMENT_3D('',#5307,#4273,#4274);
#3583=AXIS2_PLACEMENT_3D('',#5309,#4276,#4277);
#3584=AXIS2_PLACEMENT_3D('',#5311,#4278,#4279);
#3585=AXIS2_PLACEMENT_3D('',#5312,#4280,#4281);
#3586=AXIS2_PLACEMENT_3D('',#5314,#4282,#4283);
#3587=AXIS2_PLACEMENT_3D('',#5316,#4285,#4286);
#3588=AXIS2_PLACEMENT_3D('',#5318,#4288,#4289);
#3589=AXIS2_PLACEMENT_3D('',#5319,#4290,#4291);
#3590=AXIS2_PLACEMENT_3D('',#5321,#4292,#4293);
#3591=AXIS2_PLACEMENT_3D('',#5324,#4295,#4296);
#3592=AXIS2_PLACEMENT_3D('',#5325,#4297,#4298);
#3593=AXIS2_PLACEMENT_3D('',#5327,#4299,#4300);
#3594=AXIS2_PLACEMENT_3D('',#5330,#4302,#4303);
#3595=AXIS2_PLACEMENT_3D('',#5331,#4304,#4305);
#3596=AXIS2_PLACEMENT_3D('',#5332,#4306,#4307);
#3597=AXIS2_PLACEMENT_3D('',#5333,#4308,#4309);
#3598=AXIS2_PLACEMENT_3D('',#5334,#4310,#4311);
#3599=AXIS2_PLACEMENT_3D('',#5336,#4312,#4313);
#3600=AXIS2_PLACEMENT_3D('',#5339,#4315,#4316);
#3601=AXIS2_PLACEMENT_3D('',#5340,#4317,#4318);
#3602=AXIS2_PLACEMENT_3D('',#5342,#4319,#4320);
#3603=AXIS2_PLACEMENT_3D('',#5345,#4322,#4323);
#3604=AXIS2_PLACEMENT_3D('',#5346,#4324,#4325);
#3605=AXIS2_PLACEMENT_3D('',#5347,#4326,#4327);
#3606=AXIS2_PLACEMENT_3D('',#5348,#4328,#4329);
#3607=AXIS2_PLACEMENT_3D('',#5349,#4330,#4331);
#3608=AXIS2_PLACEMENT_3D('',#5350,#4332,#4333);
#3609=AXIS2_PLACEMENT_3D('',#5353,#4334,#4335);
#3610=AXIS2_PLACEMENT_3D('',#5354,#4336,#4337);
#3611=AXIS2_PLACEMENT_3D('',#5356,#4338,#4339);
#3612=AXIS2_PLACEMENT_3D('',#5358,#4340,#4341);
#3613=AXIS2_PLACEMENT_3D('',#5359,#4342,#4343);
#3614=AXIS2_PLACEMENT_3D('',#5360,#4344,#4345);
#3615=AXIS2_PLACEMENT_3D('',#5363,#4347,#4348);
#3616=AXIS2_PLACEMENT_3D('',#5364,#4349,#4350);
#3617=AXIS2_PLACEMENT_3D('',#5366,#4351,#4352);
#3618=AXIS2_PLACEMENT_3D('',#5369,#4354,#4355);
#3619=AXIS2_PLACEMENT_3D('',#5370,#4356,#4357);
#3620=AXIS2_PLACEMENT_3D('',#5373,#4359,#4360);
#3621=AXIS2_PLACEMENT_3D('',#5374,#4361,#4362);
#3622=AXIS2_PLACEMENT_3D('',#5375,#4363,#4364);
#3623=AXIS2_PLACEMENT_3D('',#5377,#4365,#4366);
#3624=AXIS2_PLACEMENT_3D('',#5379,#4368,#4369);
#3625=AXIS2_PLACEMENT_3D('',#5381,#4370,#4371);
#3626=AXIS2_PLACEMENT_3D('',#5382,#4372,#4373);
#3627=AXIS2_PLACEMENT_3D('',#5384,#4375,#4376);
#3628=AXIS2_PLACEMENT_3D('',#5385,#4377,#4378);
#3629=AXIS2_PLACEMENT_3D('',#5388,#4379,#4380);
#3630=AXIS2_PLACEMENT_3D('',#5389,#4381,#4382);
#3631=AXIS2_PLACEMENT_3D('',#5391,#4383,#4384);
#3632=AXIS2_PLACEMENT_3D('',#5393,#4385,#4386);
#3633=AXIS2_PLACEMENT_3D('',#5394,#4387,#4388);
#3634=AXIS2_PLACEMENT_3D('',#5395,#4389,#4390);
#3635=AXIS2_PLACEMENT_3D('',#5397,#4391,#4392);
#3636=AXIS2_PLACEMENT_3D('',#5399,#4394,#4395);
#3637=AXIS2_PLACEMENT_3D('',#5401,#4396,#4397);
#3638=AXIS2_PLACEMENT_3D('',#5403,#4398,#4399);
#3639=AXIS2_PLACEMENT_3D('',#5404,#4400,#4401);
#3640=AXIS2_PLACEMENT_3D('',#5406,#4402,#4403);
#3641=AXIS2_PLACEMENT_3D('',#5408,#4405,#4406);
#3642=AXIS2_PLACEMENT_3D('',#5410,#4407,#4408);
#3643=AXIS2_PLACEMENT_3D('',#5412,#4410,#4411);
#3644=AXIS2_PLACEMENT_3D('',#5414,#4412,#4413);
#3645=AXIS2_PLACEMENT_3D('',#5416,#4415,#4416);
#3646=AXIS2_PLACEMENT_3D('',#5417,#4417,#4418);
#3647=AXIS2_PLACEMENT_3D('',#5419,#4420,#4421);
#3648=AXIS2_PLACEMENT_3D('',#5420,#4422,#4423);
#3649=AXIS2_PLACEMENT_3D('',#5423,#4424,#4425);
#3650=AXIS2_PLACEMENT_3D('',#5424,#4426,#4427);
#3651=AXIS2_PLACEMENT_3D('',#5427,#4428,#4429);
#3652=AXIS2_PLACEMENT_3D('',#5428,#4430,#4431);
#3653=AXIS2_PLACEMENT_3D('',#5431,#4432,#4433);
#3654=AXIS2_PLACEMENT_3D('',#5432,#4434,#4435);
#3655=AXIS2_PLACEMENT_3D('',#5435,#4436,#4437);
#3656=AXIS2_PLACEMENT_3D('',#5436,#4438,#4439);
#3657=AXIS2_PLACEMENT_3D('',#5439,#4440,#4441);
#3658=AXIS2_PLACEMENT_3D('',#5440,#4442,#4443);
#3659=AXIS2_PLACEMENT_3D('',#5443,#4444,#4445);
#3660=AXIS2_PLACEMENT_3D('',#5444,#4446,#4447);
#3661=AXIS2_PLACEMENT_3D('',#5447,#4448,#4449);
#3662=AXIS2_PLACEMENT_3D('',#5448,#4450,#4451);
#3663=AXIS2_PLACEMENT_3D('',#5451,#4452,#4453);
#3664=AXIS2_PLACEMENT_3D('',#5452,#4454,#4455);
#3665=AXIS2_PLACEMENT_3D('',#5453,#4456,#4457);
#3666=AXIS2_PLACEMENT_3D('',#5479,#4458,#4459);
#3667=AXIS2_PLACEMENT_3D('',#5503,#4460,#4461);
#3668=AXIS2_PLACEMENT_3D('',#5504,#4462,#4463);
#3669=AXIS2_PLACEMENT_3D('',#5506,#4464,#4465);
#3670=AXIS2_PLACEMENT_3D('',#5531,#4466,#4467);
#3671=AXIS2_PLACEMENT_3D('',#5556,#4468,#4469);
#3672=AXIS2_PLACEMENT_3D('',#5572,#4471,#4472);
#3673=AXIS2_PLACEMENT_3D('',#5587,#4473,#4474);
#3674=AXIS2_PLACEMENT_3D('',#5612,#4475,#4476);
#3675=AXIS2_PLACEMENT_3D('',#5637,#4477,#4478);
#3676=AXIS2_PLACEMENT_3D('',#5662,#4479,#4480);
#3677=AXIS2_PLACEMENT_3D('',#5686,#4481,#4482);
#3678=AXIS2_PLACEMENT_3D('',#5687,#4483,#4484);
#3679=AXIS2_PLACEMENT_3D('',#5689,#4485,#4486);
#3680=AXIS2_PLACEMENT_3D('',#5690,#4487,#4488);
#3681=AXIS2_PLACEMENT_3D('',#5691,#4489,#4490);
#3682=AXIS2_PLACEMENT_3D('',#5715,#4491,#4492);
#3683=AXIS2_PLACEMENT_3D('',#5716,#4493,#4494);
#3684=AXIS2_PLACEMENT_3D('',#5718,#4495,#4496);
#3685=AXIS2_PLACEMENT_3D('',#5719,#4497,#4498);
#3686=AXIS2_PLACEMENT_3D('',#5720,#4499,#4500);
#3687=AXIS2_PLACEMENT_3D('',#5744,#4501,#4502);
#3688=AXIS2_PLACEMENT_3D('',#5745,#4503,#4504);
#3689=AXIS2_PLACEMENT_3D('',#5747,#4505,#4506);
#3690=AXIS2_PLACEMENT_3D('',#5748,#4507,#4508);
#3691=AXIS2_PLACEMENT_3D('',#5749,#4509,#4510);
#3692=AXIS2_PLACEMENT_3D('',#5764,#4511,#4512);
#3693=AXIS2_PLACEMENT_3D('',#5777,#4513,#4514);
#3694=AXIS2_PLACEMENT_3D('',#5779,#4515,#4516);
#3695=AXIS2_PLACEMENT_3D('',#5780,#4517,#4518);
#3696=AXIS2_PLACEMENT_3D('',#5781,#4519,#4520);
#3697=AXIS2_PLACEMENT_3D('',#5805,#4521,#4522);
#3698=AXIS2_PLACEMENT_3D('',#5806,#4523,#4524);
#3699=AXIS2_PLACEMENT_3D('',#5808,#4525,#4526);
#3700=AXIS2_PLACEMENT_3D('',#5809,#4527,#4528);
#3701=AXIS2_PLACEMENT_3D('',#5810,#4529,#4530);
#3702=AXIS2_PLACEMENT_3D('',#5834,#4531,#4532);
#3703=AXIS2_PLACEMENT_3D('',#5835,#4533,#4534);
#3704=AXIS2_PLACEMENT_3D('',#5837,#4535,#4536);
#3705=AXIS2_PLACEMENT_3D('',#5838,#4537,#4538);
#3706=AXIS2_PLACEMENT_3D('',#5839,#4539,#4540);
#3707=AXIS2_PLACEMENT_3D('',#5863,#4541,#4542);
#3708=AXIS2_PLACEMENT_3D('',#5864,#4543,#4544);
#3709=AXIS2_PLACEMENT_3D('',#5866,#4545,#4546);
#3710=AXIS2_PLACEMENT_3D('',#5869,#4548,#4549);
#3711=AXIS2_PLACEMENT_3D('',#5893,#4550,#4551);
#3712=AXIS2_PLACEMENT_3D('',#5894,#4552,#4553);
#3713=AXIS2_PLACEMENT_3D('',#5895,#4554,#4555);
#3714=AXIS2_PLACEMENT_3D('',#5896,#4556,#4557);
#3715=AXIS2_PLACEMENT_3D('',#5897,#4558,#4559);
#3716=AXIS2_PLACEMENT_3D('',#5898,#4560,#4561);
#3717=AXIS2_PLACEMENT_3D('',#5899,#4562,#4563);
#3718=AXIS2_PLACEMENT_3D('',#5900,#4564,#4565);
#3719=AXIS2_PLACEMENT_3D('',#5901,#4566,#4567);
#3720=AXIS2_PLACEMENT_3D('',#5903,#4568,#4569);
#3721=AXIS2_PLACEMENT_3D('',#5905,#4570,#4571);
#3722=AXIS2_PLACEMENT_3D('',#5906,#4572,#4573);
#3723=AXIS2_PLACEMENT_3D('',#5908,#4574,#4575);
#3724=AXIS2_PLACEMENT_3D('',#5910,#4577,#4578);
#3725=AXIS2_PLACEMENT_3D('',#5912,#4579,#4580);
#3726=AXIS2_PLACEMENT_3D('',#5913,#4581,#4582);
#3727=AXIS2_PLACEMENT_3D('',#5915,#4584,#4585);
#3728=AXIS2_PLACEMENT_3D('',#5917,#4586,#4587);
#3729=AXIS2_PLACEMENT_3D('',#5919,#4588,#4589);
#3730=AXIS2_PLACEMENT_3D('',#5920,#4590,#4591);
#3731=AXIS2_PLACEMENT_3D('',#5922,#4592,#4593);
#3732=AXIS2_PLACEMENT_3D('',#5924,#4595,#4596);
#3733=AXIS2_PLACEMENT_3D('',#5926,#4597,#4598);
#3734=AXIS2_PLACEMENT_3D('',#5927,#4599,#4600);
#3735=AXIS2_PLACEMENT_3D('',#5929,#4602,#4603);
#3736=AXIS2_PLACEMENT_3D('',#5930,#4604,#4605);
#3737=AXIS2_PLACEMENT_3D('',#5931,#4606,#4607);
#3738=AXIS2_PLACEMENT_3D('',#5932,#4608,#4609);
#3739=AXIS2_PLACEMENT_3D('',#5933,#4610,#4611);
#3740=AXIS2_PLACEMENT_3D('',#5934,#4612,#4613);
#3741=AXIS2_PLACEMENT_3D('',#5935,#4614,#4615);
#3742=AXIS2_PLACEMENT_3D('',#5936,#4616,#4617);
#3743=AXIS2_PLACEMENT_3D('',#5938,#4618,#4619);
#3744=AXIS2_PLACEMENT_3D('',#5941,#4621,#4622);
#3745=AXIS2_PLACEMENT_3D('',#5942,#4623,#4624);
#3746=AXIS2_PLACEMENT_3D('',#5944,#4625,#4626);
#3747=AXIS2_PLACEMENT_3D('',#5947,#4628,#4629);
#3748=AXIS2_PLACEMENT_3D('',#5948,#4630,#4631);
#3749=AXIS2_PLACEMENT_3D('',#5950,#4632,#4633);
#3750=AXIS2_PLACEMENT_3D('',#5953,#4635,#4636);
#3751=AXIS2_PLACEMENT_3D('',#5954,#4637,#4638);
#3752=AXIS2_PLACEMENT_3D('',#5956,#4639,#4640);
#3753=AXIS2_PLACEMENT_3D('',#5959,#4642,#4643);
#3754=AXIS2_PLACEMENT_3D('',#5960,#4644,#4645);
#3755=AXIS2_PLACEMENT_3D('',#5962,#4646,#4647);
#3756=AXIS2_PLACEMENT_3D('',#5965,#4649,#4650);
#3757=AXIS2_PLACEMENT_3D('',#5966,#4651,#4652);
#3758=AXIS2_PLACEMENT_3D('',#5968,#4653,#4654);
#3759=AXIS2_PLACEMENT_3D('',#5969,#4655,#4656);
#3760=AXIS2_PLACEMENT_3D('',#5972,#4658,#4659);
#3761=AXIS2_PLACEMENT_3D('',#5973,#4660,#4661);
#3762=AXIS2_PLACEMENT_3D('',#5975,#4662,#4663);
#3763=AXIS2_PLACEMENT_3D('',#5978,#4665,#4666);
#3764=AXIS2_PLACEMENT_3D('',#5979,#4667,#4668);
#3765=AXIS2_PLACEMENT_3D('',#5980,#4669,#4670);
#3766=AXIS2_PLACEMENT_3D('',#5981,#4671,#4672);
#3767=AXIS2_PLACEMENT_3D('',#5982,#4673,#4674);
#3768=AXIS2_PLACEMENT_3D('',#5984,#4675,#4676);
#3769=AXIS2_PLACEMENT_3D('',#5987,#4678,#4679);
#3770=AXIS2_PLACEMENT_3D('',#5988,#4680,#4681);
#3771=AXIS2_PLACEMENT_3D('',#5990,#4682,#4683);
#3772=AXIS2_PLACEMENT_3D('',#5993,#4685,#4686);
#3773=AXIS2_PLACEMENT_3D('',#5994,#4687,#4688);
#3774=AXIS2_PLACEMENT_3D('',#5996,#4689,#4690);
#3775=AXIS2_PLACEMENT_3D('',#5999,#4692,#4693);
#3776=AXIS2_PLACEMENT_3D('',#6000,#4694,#4695);
#3777=AXIS2_PLACEMENT_3D('',#6002,#4696,#4697);
#3778=AXIS2_PLACEMENT_3D('',#6005,#4699,#4700);
#3779=AXIS2_PLACEMENT_3D('',#6006,#4701,#4702);
#3780=AXIS2_PLACEMENT_3D('',#6008,#4703,#4704);
#3781=AXIS2_PLACEMENT_3D('',#6011,#4706,#4707);
#3782=AXIS2_PLACEMENT_3D('',#6012,#4708,#4709);
#3783=AXIS2_PLACEMENT_3D('',#6014,#4710,#4711);
#3784=AXIS2_PLACEMENT_3D('',#6015,#4712,#4713);
#3785=AXIS2_PLACEMENT_3D('',#6017,#4714,#4715);
#3786=AXIS2_PLACEMENT_3D('',#6019,#4717,#4718);
#3787=AXIS2_PLACEMENT_3D('',#6021,#4719,#4720);
#3788=AXIS2_PLACEMENT_3D('',#6024,#4722,#4723);
#3789=AXIS2_PLACEMENT_3D('',#6025,#4724,#4725);
#3790=AXIS2_PLACEMENT_3D('',#6026,#4726,#4727);
#3791=AXIS2_PLACEMENT_3D('',#6027,#4728,#4729);
#3792=AXIS2_PLACEMENT_3D('',#6028,#4730,#4731);
#3793=AXIS2_PLACEMENT_3D('',#6030,#4732,#4733);
#3794=AXIS2_PLACEMENT_3D('',#6033,#4735,#4736);
#3795=AXIS2_PLACEMENT_3D('',#6034,#4737,#4738);
#3796=AXIS2_PLACEMENT_3D('',#6036,#4739,#4740);
#3797=AXIS2_PLACEMENT_3D('',#6039,#4742,#4743);
#3798=AXIS2_PLACEMENT_3D('',#6040,#4744,#4745);
#3799=AXIS2_PLACEMENT_3D('',#6041,#4746,#4747);
#3800=AXIS2_PLACEMENT_3D('',#6042,#4748,#4749);
#3801=AXIS2_PLACEMENT_3D('',#6043,#4750,#4751);
#3802=AXIS2_PLACEMENT_3D('',#6045,#4752,#4753);
#3803=AXIS2_PLACEMENT_3D('',#6048,#4755,#4756);
#3804=AXIS2_PLACEMENT_3D('',#6049,#4757,#4758);
#3805=AXIS2_PLACEMENT_3D('',#6051,#4759,#4760);
#3806=AXIS2_PLACEMENT_3D('',#6054,#4762,#4763);
#3807=AXIS2_PLACEMENT_3D('',#6055,#4764,#4765);
#3808=AXIS2_PLACEMENT_3D('',#6057,#4766,#4767);
#3809=AXIS2_PLACEMENT_3D('',#6060,#4769,#4770);
#3810=AXIS2_PLACEMENT_3D('',#6061,#4771,#4772);
#3811=AXIS2_PLACEMENT_3D('',#6063,#4773,#4774);
#3812=AXIS2_PLACEMENT_3D('',#6066,#4776,#4777);
#3813=AXIS2_PLACEMENT_3D('',#6067,#4778,#4779);
#3814=AXIS2_PLACEMENT_3D('',#6069,#4780,#4781);
#3815=AXIS2_PLACEMENT_3D('',#6072,#4783,#4784);
#3816=AXIS2_PLACEMENT_3D('',#6073,#4785,#4786);
#3817=AXIS2_PLACEMENT_3D('',#6075,#4787,#4788);
#3818=AXIS2_PLACEMENT_3D('',#6078,#4790,#4791);
#3819=AXIS2_PLACEMENT_3D('',#6079,#4792,#4793);
#3820=AXIS2_PLACEMENT_3D('',#6080,#4794,#4795);
#3821=AXIS2_PLACEMENT_3D('',#6081,#4796,#4797);
#3822=AXIS2_PLACEMENT_3D('',#6082,#4798,#4799);
#3823=AXIS2_PLACEMENT_3D('',#6084,#4800,#4801);
#3824=AXIS2_PLACEMENT_3D('',#6085,#4802,#4803);
#3825=AXIS2_PLACEMENT_3D('',#6087,#4804,#4805);
#3826=AXIS2_PLACEMENT_3D('',#6089,#4807,#4808);
#3827=AXIS2_PLACEMENT_3D('',#6091,#4809,#4810);
#3828=AXIS2_PLACEMENT_3D('',#6093,#4812,#4813);
#3829=AXIS2_PLACEMENT_3D('',#6095,#4814,#4815);
#3830=AXIS2_PLACEMENT_3D('',#6097,#4817,#4818);
#3831=AXIS2_PLACEMENT_3D('',#6099,#4819,#4820);
#3832=AXIS2_PLACEMENT_3D('',#6100,#4821,#4822);
#3833=AXIS2_PLACEMENT_3D('',#6102,#4823,#4824);
#3834=AXIS2_PLACEMENT_3D('',#6104,#4826,#4827);
#3835=AXIS2_PLACEMENT_3D('',#6106,#4828,#4829);
#3836=AXIS2_PLACEMENT_3D('',#6108,#4831,#4832);
#3837=AXIS2_PLACEMENT_3D('',#6110,#4833,#4834);
#3838=AXIS2_PLACEMENT_3D('',#6112,#4836,#4837);
#3839=AXIS2_PLACEMENT_3D('',#6113,#4838,#4839);
#3840=AXIS2_PLACEMENT_3D('',#6122,#4844,#4845);
#3841=AXIS2_PLACEMENT_3D('',#6128,#4849,#4850);
#3842=AXIS2_PLACEMENT_3D('',#6134,#4854,#4855);
#3843=AXIS2_PLACEMENT_3D('',#6140,#4859,#4860);
#3844=AXIS2_PLACEMENT_3D('',#6146,#4864,#4865);
#3845=AXIS2_PLACEMENT_3D('',#6149,#4868,#4869);
#3846=AXIS2_PLACEMENT_3D('',#6150,#4870,#4871);
#3847=AXIS2_PLACEMENT_3D('',#6151,#4872,#4873);
#3848=AXIS2_PLACEMENT_3D('',#6152,#4874,#4875);
#3849=AXIS2_PLACEMENT_3D('',#6153,#4876,#4877);
#3850=AXIS2_PLACEMENT_3D('',#6154,#4878,#4879);
#3851=AXIS2_PLACEMENT_3D('',#6155,#4880,#4881);
#3852=AXIS2_PLACEMENT_3D('',#6156,#4882,#4883);
#3853=AXIS2_PLACEMENT_3D('',#6157,#4884,#4885);
#3854=AXIS2_PLACEMENT_3D('',#6158,#4886,#4887);
#3855=AXIS2_PLACEMENT_3D('',#6159,#4888,#4889);
#3856=AXIS2_PLACEMENT_3D('',#6160,#4890,#4891);
#3857=AXIS2_PLACEMENT_3D('',#6161,#4892,#4893);
#3858=AXIS2_PLACEMENT_3D('',#6162,#4894,#4895);
#3859=AXIS2_PLACEMENT_3D('',#6163,#4896,#4897);
#3860=AXIS2_PLACEMENT_3D('',#6164,#4898,#4899);
#3861=AXIS2_PLACEMENT_3D('',#6165,#4900,#4901);
#3862=AXIS2_PLACEMENT_3D('',#6166,#4902,#4903);
#3863=AXIS2_PLACEMENT_3D('',#6167,#4904,#4905);
#3864=AXIS2_PLACEMENT_3D('',#6168,#4906,#4907);
#3865=AXIS2_PLACEMENT_3D('',#6169,#4908,#4909);
#3866=AXIS2_PLACEMENT_3D('',#6170,#4910,#4911);
#3867=AXIS2_PLACEMENT_3D('',#6171,#4912,#4913);
#3868=AXIS2_PLACEMENT_3D('',#6172,#4914,#4915);
#3869=AXIS2_PLACEMENT_3D('',#6173,#4916,#4917);
#3870=AXIS2_PLACEMENT_3D('',#6174,#4918,#4919);
#3871=AXIS2_PLACEMENT_3D('',#6175,#4920,#4921);
#3872=AXIS2_PLACEMENT_3D('',#6176,#4922,#4923);
#3873=AXIS2_PLACEMENT_3D('',#6177,#4924,#4925);
#3874=AXIS2_PLACEMENT_3D('',#6178,#4926,#4927);
#3875=AXIS2_PLACEMENT_3D('',#6179,#4928,#4929);
#3876=AXIS2_PLACEMENT_3D('',#6180,#4930,#4931);
#3877=AXIS2_PLACEMENT_3D('',#6181,#4932,#4933);
#3878=AXIS2_PLACEMENT_3D('',#6182,#4934,#4935);
#3879=AXIS2_PLACEMENT_3D('',#6183,#4936,#4937);
#3880=AXIS2_PLACEMENT_3D('',#6184,#4938,#4939);
#3881=AXIS2_PLACEMENT_3D('',#6185,#4940,#4941);
#3882=AXIS2_PLACEMENT_3D('',#6186,#4942,#4943);
#3883=AXIS2_PLACEMENT_3D('',#6187,#4944,#4945);
#3884=AXIS2_PLACEMENT_3D('',#6188,#4946,#4947);
#3885=AXIS2_PLACEMENT_3D('',#6189,#4948,#4949);
#3886=DIRECTION('axis',(0.,0.,1.));
#3887=DIRECTION('refdir',(1.,0.,0.));
#3888=DIRECTION('axis',(0.,0.,1.));
#3889=DIRECTION('refdir',(1.,0.,0.));
#3890=DIRECTION('axis',(0.,0.,1.));
#3891=DIRECTION('refdir',(1.,0.,0.));
#3892=DIRECTION('center_axis',(0.,0.,1.));
#3893=DIRECTION('ref_axis',(1.,0.,0.));
#3894=DIRECTION('center_axis',(0.,0.,1.));
#3895=DIRECTION('ref_axis',(1.,0.,0.));
#3896=DIRECTION('',(0.,0.,1.));
#3897=DIRECTION('center_axis',(0.,0.,-1.));
#3898=DIRECTION('ref_axis',(1.,0.,0.));
#3899=DIRECTION('center_axis',(0.,0.,1.));
#3900=DIRECTION('ref_axis',(1.,0.,0.));
#3901=DIRECTION('center_axis',(0.,0.,1.));
#3902=DIRECTION('ref_axis',(1.,0.,0.));
#3903=DIRECTION('',(0.,0.,1.));
#3904=DIRECTION('center_axis',(0.,0.,-1.));
#3905=DIRECTION('ref_axis',(1.,0.,0.));
#3906=DIRECTION('center_axis',(0.,1.,0.));
#3907=DIRECTION('ref_axis',(1.,0.,0.));
#3908=DIRECTION('center_axis',(0.,1.,0.));
#3909=DIRECTION('ref_axis',(1.,0.,0.));
#3910=DIRECTION('',(0.,1.,0.));
#3911=DIRECTION('center_axis',(0.,-1.,0.));
#3912=DIRECTION('ref_axis',(1.,0.,0.));
#3913=DIRECTION('center_axis',(0.,0.,1.));
#3914=DIRECTION('ref_axis',(1.,0.,0.));
#3915=DIRECTION('',(-1.,0.,0.));
#3916=DIRECTION('',(0.,1.,0.));
#3917=DIRECTION('',(1.,0.,0.));
#3918=DIRECTION('',(0.,1.,0.));
#3919=DIRECTION('',(-1.,0.,0.));
#3920=DIRECTION('',(0.,1.,0.));
#3921=DIRECTION('',(1.,0.,0.));
#3922=DIRECTION('',(0.,-1.,0.));
#3923=DIRECTION('center_axis',(-1.,0.,0.));
#3924=DIRECTION('ref_axis',(0.,0.,1.));
#3925=DIRECTION('',(0.,0.,-1.));
#3926=DIRECTION('',(0.,0.,1.));
#3927=DIRECTION('',(0.,1.,0.));
#3928=DIRECTION('center_axis',(1.,0.,0.));
#3929=DIRECTION('ref_axis',(0.,0.,-1.));
#3930=DIRECTION('',(0.,0.,1.));
#3931=DIRECTION('',(0.,1.,0.));
#3932=DIRECTION('',(0.,0.,-1.));
#3933=DIRECTION('center_axis',(0.,1.,0.));
#3934=DIRECTION('ref_axis',(0.,0.,1.));
#3935=DIRECTION('',(-1.,0.,0.));
#3936=DIRECTION('center_axis',(0.,1.,0.));
#3937=DIRECTION('ref_axis',(1.,0.,0.));
#3938=DIRECTION('',(1.,0.,0.));
#3939=DIRECTION('center_axis',(0.,-1.,0.));
#3940=DIRECTION('ref_axis',(1.,0.,0.));
#3941=DIRECTION('',(0.,0.,1.));
#3942=DIRECTION('',(1.,0.,0.));
#3943=DIRECTION('',(0.,0.,1.));
#3944=DIRECTION('center_axis',(1.,0.,0.));
#3945=DIRECTION('ref_axis',(0.,1.,0.));
#3946=DIRECTION('',(0.,0.,1.));
#3947=DIRECTION('',(0.,1.,0.));
#3948=DIRECTION('center_axis',(0.,1.,0.));
#3949=DIRECTION('ref_axis',(-1.,0.,0.));
#3950=DIRECTION('',(0.,0.,1.));
#3951=DIRECTION('',(-1.,0.,0.));
#3952=DIRECTION('center_axis',(-1.,0.,0.));
#3953=DIRECTION('ref_axis',(0.,-1.,0.));
#3954=DIRECTION('',(0.,-1.,0.));
#3955=DIRECTION('center_axis',(0.,0.,1.));
#3956=DIRECTION('ref_axis',(1.,0.,0.));
#3957=DIRECTION('center_axis',(0.,0.,1.));
#3958=DIRECTION('ref_axis',(1.,0.,0.));
#3959=DIRECTION('axis',(0.,0.,1.));
#3960=DIRECTION('refdir',(1.,0.,0.));
#3961=DIRECTION('center_axis',(0.,0.,1.));
#3962=DIRECTION('ref_axis',(1.,0.,0.));
#3963=DIRECTION('center_axis',(0.,0.,1.));
#3964=DIRECTION('ref_axis',(1.,0.,0.));
#3965=DIRECTION('',(0.,0.,1.));
#3966=DIRECTION('center_axis',(0.,0.,-1.));
#3967=DIRECTION('ref_axis',(1.,0.,0.));
#3968=DIRECTION('center_axis',(0.,0.,1.));
#3969=DIRECTION('ref_axis',(1.,0.,0.));
#3970=DIRECTION('center_axis',(0.,0.,1.));
#3971=DIRECTION('ref_axis',(1.,0.,0.));
#3972=DIRECTION('',(0.,0.,1.));
#3973=DIRECTION('center_axis',(0.,0.,-1.));
#3974=DIRECTION('ref_axis',(1.,0.,0.));
#3975=DIRECTION('center_axis',(0.,1.,0.));
#3976=DIRECTION('ref_axis',(1.,0.,0.));
#3977=DIRECTION('center_axis',(0.,1.,0.));
#3978=DIRECTION('ref_axis',(1.,0.,0.));
#3979=DIRECTION('',(0.,1.,0.));
#3980=DIRECTION('center_axis',(0.,-1.,0.));
#3981=DIRECTION('ref_axis',(1.,0.,0.));
#3982=DIRECTION('center_axis',(0.,0.,1.));
#3983=DIRECTION('ref_axis',(1.,0.,0.));
#3984=DIRECTION('',(-1.,0.,0.));
#3985=DIRECTION('',(0.,1.,0.));
#3986=DIRECTION('',(1.,0.,0.));
#3987=DIRECTION('',(0.,1.,0.));
#3988=DIRECTION('',(-1.,0.,0.));
#3989=DIRECTION('',(0.,1.,0.));
#3990=DIRECTION('',(1.,0.,0.));
#3991=DIRECTION('',(0.,-1.,0.));
#3992=DIRECTION('center_axis',(-1.,0.,0.));
#3993=DIRECTION('ref_axis',(0.,0.,1.));
#3994=DIRECTION('',(0.,0.,-1.));
#3995=DIRECTION('',(0.,0.,1.));
#3996=DIRECTION('',(0.,1.,0.));
#3997=DIRECTION('center_axis',(1.,0.,0.));
#3998=DIRECTION('ref_axis',(0.,0.,-1.));
#3999=DIRECTION('',(0.,0.,1.));
#4000=DIRECTION('',(0.,1.,0.));
#4001=DIRECTION('',(0.,0.,-1.));
#4002=DIRECTION('center_axis',(0.,1.,0.));
#4003=DIRECTION('ref_axis',(0.,0.,1.));
#4004=DIRECTION('',(-1.,0.,0.));
#4005=DIRECTION('center_axis',(0.,1.,0.));
#4006=DIRECTION('ref_axis',(1.,0.,0.));
#4007=DIRECTION('',(1.,0.,0.));
#4008=DIRECTION('center_axis',(0.,-1.,0.));
#4009=DIRECTION('ref_axis',(1.,0.,0.));
#4010=DIRECTION('',(0.,0.,1.));
#4011=DIRECTION('',(1.,0.,0.));
#4012=DIRECTION('',(0.,0.,1.));
#4013=DIRECTION('center_axis',(1.,0.,0.));
#4014=DIRECTION('ref_axis',(0.,1.,0.));
#4015=DIRECTION('',(0.,0.,1.));
#4016=DIRECTION('',(0.,1.,0.));
#4017=DIRECTION('center_axis',(0.,1.,0.));
#4018=DIRECTION('ref_axis',(-1.,0.,0.));
#4019=DIRECTION('',(0.,0.,1.));
#4020=DIRECTION('',(-1.,0.,0.));
#4021=DIRECTION('center_axis',(-1.,0.,0.));
#4022=DIRECTION('ref_axis',(0.,-1.,0.));
#4023=DIRECTION('',(0.,-1.,0.));
#4024=DIRECTION('center_axis',(0.,0.,1.));
#4025=DIRECTION('ref_axis',(1.,0.,0.));
#4026=DIRECTION('center_axis',(0.,0.,1.));
#4027=DIRECTION('ref_axis',(1.,0.,0.));
#4028=DIRECTION('axis',(0.,0.,1.));
#4029=DIRECTION('refdir',(1.,0.,0.));
#4030=DIRECTION('center_axis',(0.,1.,0.));
#4031=DIRECTION('ref_axis',(1.,0.,0.));
#4032=DIRECTION('center_axis',(0.,1.,0.));
#4033=DIRECTION('ref_axis',(1.,0.,0.));
#4034=DIRECTION('',(0.,1.,0.));
#4035=DIRECTION('center_axis',(0.,-1.,0.));
#4036=DIRECTION('ref_axis',(1.,0.,0.));
#4037=DIRECTION('center_axis',(0.,1.,0.));
#4038=DIRECTION('ref_axis',(1.,0.,0.));
#4039=DIRECTION('center_axis',(0.,1.,0.));
#4040=DIRECTION('ref_axis',(1.,0.,0.));
#4041=DIRECTION('center_axis',(0.,1.,0.));
#4042=DIRECTION('ref_axis',(1.,0.,0.));
#4043=DIRECTION('',(0.,1.,0.));
#4044=DIRECTION('center_axis',(0.,1.,0.));
#4045=DIRECTION('ref_axis',(1.,0.,0.));
#4046=DIRECTION('center_axis',(0.,1.,0.));
#4047=DIRECTION('ref_axis',(1.,0.,0.));
#4048=DIRECTION('center_axis',(0.,1.,0.));
#4049=DIRECTION('ref_axis',(1.,0.,0.));
#4050=DIRECTION('center_axis',(0.,1.,0.));
#4051=DIRECTION('ref_axis',(1.,0.,0.));
#4052=DIRECTION('center_axis',(0.,1.,0.));
#4053=DIRECTION('ref_axis',(1.,0.,0.));
#4054=DIRECTION('center_axis',(0.,1.,0.));
#4055=DIRECTION('ref_axis',(1.,0.,0.));
#4056=DIRECTION('center_axis',(0.,1.,0.));
#4057=DIRECTION('ref_axis',(1.,0.,0.));
#4058=DIRECTION('center_axis',(0.,-1.,0.));
#4059=DIRECTION('ref_axis',(1.,0.,0.));
#4060=DIRECTION('center_axis',(0.,1.,0.));
#4061=DIRECTION('ref_axis',(1.,0.,0.));
#4062=DIRECTION('',(0.,-1.,0.));
#4063=DIRECTION('center_axis',(0.,1.,0.));
#4064=DIRECTION('ref_axis',(1.,0.,0.));
#4065=DIRECTION('',(0.,-1.,0.));
#4066=DIRECTION('center_axis',(0.,1.,0.));
#4067=DIRECTION('ref_axis',(1.,0.,0.));
#4068=DIRECTION('center_axis',(0.,1.,0.));
#4069=DIRECTION('ref_axis',(1.,0.,0.));
#4070=DIRECTION('center_axis',(0.,1.,0.));
#4071=DIRECTION('ref_axis',(1.,0.,0.));
#4072=DIRECTION('',(0.,-1.,0.));
#4073=DIRECTION('center_axis',(0.,1.,0.));
#4074=DIRECTION('ref_axis',(1.,0.,0.));
#4075=DIRECTION('center_axis',(0.,1.,0.));
#4076=DIRECTION('ref_axis',(1.,0.,0.));
#4077=DIRECTION('axis',(0.,0.,1.));
#4078=DIRECTION('refdir',(1.,0.,0.));
#4079=DIRECTION('center_axis',(0.,1.,0.));
#4080=DIRECTION('ref_axis',(1.,0.,0.));
#4081=DIRECTION('center_axis',(0.,-1.,0.));
#4082=DIRECTION('ref_axis',(1.,0.,0.));
#4083=DIRECTION('',(0.,-1.,0.));
#4084=DIRECTION('center_axis',(0.,-1.,0.));
#4085=DIRECTION('ref_axis',(1.,0.,0.));
#4086=DIRECTION('center_axis',(0.,1.,0.));
#4087=DIRECTION('ref_axis',(1.,0.,0.));
#4088=DIRECTION('center_axis',(0.,1.,0.));
#4089=DIRECTION('ref_axis',(1.,0.,0.));
#4090=DIRECTION('',(0.,-1.,0.));
#4091=DIRECTION('center_axis',(0.,1.,0.));
#4092=DIRECTION('ref_axis',(1.,0.,0.));
#4093=DIRECTION('center_axis',(0.,1.,0.));
#4094=DIRECTION('ref_axis',(1.,0.,0.));
#4095=DIRECTION('center_axis',(0.,1.,0.));
#4096=DIRECTION('ref_axis',(1.,0.,0.));
#4097=DIRECTION('axis',(0.,0.,1.));
#4098=DIRECTION('refdir',(1.,0.,0.));
#4099=DIRECTION('center_axis',(0.,1.,0.));
#4100=DIRECTION('ref_axis',(1.,0.,0.));
#4101=DIRECTION('center_axis',(0.,-1.,0.));
#4102=DIRECTION('ref_axis',(1.,0.,0.));
#4103=DIRECTION('',(0.,-1.,0.));
#4104=DIRECTION('center_axis',(0.,-1.,0.));
#4105=DIRECTION('ref_axis',(1.,0.,0.));
#4106=DIRECTION('center_axis',(0.,1.,0.));
#4107=DIRECTION('ref_axis',(1.,0.,0.));
#4108=DIRECTION('center_axis',(0.,1.,0.));
#4109=DIRECTION('ref_axis',(1.,0.,0.));
#4110=DIRECTION('',(0.,-1.,0.));
#4111=DIRECTION('center_axis',(0.,1.,0.));
#4112=DIRECTION('ref_axis',(1.,0.,0.));
#4113=DIRECTION('center_axis',(0.,1.,0.));
#4114=DIRECTION('ref_axis',(1.,0.,0.));
#4115=DIRECTION('center_axis',(0.,1.,0.));
#4116=DIRECTION('ref_axis',(1.,0.,0.));
#4117=DIRECTION('axis',(0.,0.,1.));
#4118=DIRECTION('refdir',(1.,0.,0.));
#4119=DIRECTION('center_axis',(0.,0.,1.));
#4120=DIRECTION('ref_axis',(1.,0.,0.));
#4121=DIRECTION('center_axis',(0.,0.,1.));
#4122=DIRECTION('ref_axis',(1.,0.,0.));
#4123=DIRECTION('',(0.,0.,1.));
#4124=DIRECTION('center_axis',(0.,0.,-1.));
#4125=DIRECTION('ref_axis',(1.,0.,0.));
#4126=DIRECTION('center_axis',(0.,0.,1.));
#4127=DIRECTION('ref_axis',(1.,0.,0.));
#4128=DIRECTION('center_axis',(0.,0.,1.));
#4129=DIRECTION('ref_axis',(1.,0.,0.));
#4130=DIRECTION('',(0.,0.,1.));
#4131=DIRECTION('center_axis',(0.,0.,-1.));
#4132=DIRECTION('ref_axis',(1.,0.,0.));
#4133=DIRECTION('center_axis',(0.,0.,1.));
#4134=DIRECTION('ref_axis',(1.,0.,0.));
#4135=DIRECTION('center_axis',(0.,0.,1.));
#4136=DIRECTION('ref_axis',(1.,0.,0.));
#4137=DIRECTION('',(0.,0.,1.));
#4138=DIRECTION('center_axis',(0.,0.,-1.));
#4139=DIRECTION('ref_axis',(1.,0.,0.));
#4140=DIRECTION('center_axis',(0.,0.,1.));
#4141=DIRECTION('ref_axis',(1.,0.,0.));
#4142=DIRECTION('center_axis',(0.,0.,1.));
#4143=DIRECTION('ref_axis',(1.,0.,0.));
#4144=DIRECTION('',(0.,0.,1.));
#4145=DIRECTION('center_axis',(0.,0.,-1.));
#4146=DIRECTION('ref_axis',(1.,0.,0.));
#4147=DIRECTION('center_axis',(0.,1.,0.));
#4148=DIRECTION('ref_axis',(-1.,0.,0.));
#4149=DIRECTION('',(-1.,0.,0.));
#4150=DIRECTION('',(0.,0.,1.));
#4151=DIRECTION('',(-1.,0.,0.));
#4152=DIRECTION('',(0.,0.,1.));
#4153=DIRECTION('center_axis',(1.,0.,0.));
#4154=DIRECTION('ref_axis',(0.,1.,0.));
#4155=DIRECTION('',(0.,1.,0.));
#4156=DIRECTION('',(0.,1.,0.));
#4157=DIRECTION('',(0.,0.,1.));
#4158=DIRECTION('center_axis',(0.,-1.,0.));
#4159=DIRECTION('ref_axis',(1.,0.,0.));
#4160=DIRECTION('',(1.,0.,0.));
#4161=DIRECTION('',(1.,0.,0.));
#4162=DIRECTION('',(0.,0.,1.));
#4163=DIRECTION('center_axis',(-1.,0.,0.));
#4164=DIRECTION('ref_axis',(0.,-1.,0.));
#4165=DIRECTION('',(0.,-1.,0.));
#4166=DIRECTION('',(0.,-1.,0.));
#4167=DIRECTION('center_axis',(0.,0.,1.));
#4168=DIRECTION('ref_axis',(1.,0.,0.));
#4169=DIRECTION('center_axis',(0.,0.,1.));
#4170=DIRECTION('ref_axis',(1.,0.,0.));
#4171=DIRECTION('axis',(0.,0.,1.));
#4172=DIRECTION('refdir',(1.,0.,0.));
#4173=DIRECTION('center_axis',(0.,1.,0.));
#4174=DIRECTION('ref_axis',(-1.,0.,0.));
#4175=DIRECTION('',(-1.,0.,0.));
#4176=DIRECTION('',(0.,0.,1.));
#4177=DIRECTION('',(-1.,0.,0.));
#4178=DIRECTION('',(0.,0.,1.));
#4179=DIRECTION('center_axis',(1.,0.,0.));
#4180=DIRECTION('ref_axis',(0.,1.,0.));
#4181=DIRECTION('',(0.,1.,0.));
#4182=DIRECTION('',(0.,1.,0.));
#4183=DIRECTION('',(0.,0.,1.));
#4184=DIRECTION('center_axis',(0.,-1.,0.));
#4185=DIRECTION('ref_axis',(1.,0.,0.));
#4186=DIRECTION('',(1.,0.,0.));
#4187=DIRECTION('',(1.,0.,0.));
#4188=DIRECTION('',(0.,0.,1.));
#4189=DIRECTION('center_axis',(-1.,0.,0.));
#4190=DIRECTION('ref_axis',(0.,-1.,0.));
#4191=DIRECTION('',(0.,-1.,0.));
#4192=DIRECTION('',(0.,-1.,0.));
#4193=DIRECTION('center_axis',(0.,0.,1.));
#4194=DIRECTION('ref_axis',(1.,0.,0.));
#4195=DIRECTION('center_axis',(0.,0.,1.));
#4196=DIRECTION('ref_axis',(1.,0.,0.));
#4197=DIRECTION('axis',(0.,0.,1.));
#4198=DIRECTION('refdir',(1.,0.,0.));
#4199=DIRECTION('center_axis',(0.,1.,0.));
#4200=DIRECTION('ref_axis',(1.,0.,0.));
#4201=DIRECTION('center_axis',(0.,-1.,0.));
#4202=DIRECTION('ref_axis',(1.,0.,0.));
#4203=DIRECTION('',(0.,-1.,0.));
#4204=DIRECTION('center_axis',(0.,-1.,0.));
#4205=DIRECTION('ref_axis',(1.,0.,0.));
#4206=DIRECTION('center_axis',(0.,1.,0.));
#4207=DIRECTION('ref_axis',(1.,0.,0.));
#4208=DIRECTION('center_axis',(0.,1.,0.));
#4209=DIRECTION('ref_axis',(1.,0.,0.));
#4210=DIRECTION('',(0.,-1.,0.));
#4211=DIRECTION('center_axis',(0.,1.,0.));
#4212=DIRECTION('ref_axis',(1.,0.,0.));
#4213=DIRECTION('center_axis',(0.,1.,0.));
#4214=DIRECTION('ref_axis',(1.,0.,0.));
#4215=DIRECTION('center_axis',(0.,1.,0.));
#4216=DIRECTION('ref_axis',(1.,0.,0.));
#4217=DIRECTION('axis',(0.,0.,1.));
#4218=DIRECTION('refdir',(1.,0.,0.));
#4219=DIRECTION('center_axis',(0.866025403784439,0.,-0.5));
#4220=DIRECTION('ref_axis',(0.5,0.,0.866025403784439));
#4221=DIRECTION('',(-0.5,0.,-0.866025403784439));
#4222=DIRECTION('',(0.,-1.,0.));
#4223=DIRECTION('',(0.5,0.,0.866025403784439));
#4224=DIRECTION('',(0.,-1.,0.));
#4225=DIRECTION('center_axis',(1.92296268638356E-16,0.,-1.));
#4226=DIRECTION('ref_axis',(1.,0.,1.92296268638356E-16));
#4227=DIRECTION('',(-1.,0.,-1.92296268638356E-16));
#4228=DIRECTION('',(0.,-1.,0.));
#4229=DIRECTION('',(1.,0.,1.92296268638356E-16));
#4230=DIRECTION('center_axis',(-0.866025403784439,0.,-0.5));
#4231=DIRECTION('ref_axis',(0.5,0.,-0.866025403784439));
#4232=DIRECTION('',(-0.5,0.,0.866025403784438));
#4233=DIRECTION('',(0.,-1.,0.));
#4234=DIRECTION('',(0.5,0.,-0.866025403784438));
#4235=DIRECTION('center_axis',(-0.866025403784439,0.,0.5));
#4236=DIRECTION('ref_axis',(-0.5,0.,-0.866025403784439));
#4237=DIRECTION('',(0.5,0.,0.866025403784439));
#4238=DIRECTION('',(0.,-1.,0.));
#4239=DIRECTION('',(-0.5,0.,-0.866025403784439));
#4240=DIRECTION('center_axis',(-1.92296268638356E-16,0.,1.));
#4241=DIRECTION('ref_axis',(-1.,0.,-1.92296268638356E-16));
#4242=DIRECTION('',(1.,0.,1.92296268638356E-16));
#4243=DIRECTION('',(0.,-1.,0.));
#4244=DIRECTION('',(-1.,0.,-1.92296268638356E-16));
#4245=DIRECTION('center_axis',(0.866025403784439,0.,0.5));
#4246=DIRECTION('ref_axis',(-0.5,0.,0.866025403784439));
#4247=DIRECTION('',(0.5,0.,-0.866025403784439));
#4248=DIRECTION('',(-0.5,0.,0.866025403784439));
#4249=DIRECTION('center_axis',(0.,1.,0.));
#4250=DIRECTION('ref_axis',(1.,0.,0.));
#4251=DIRECTION('center_axis',(0.,-1.,0.));
#4252=DIRECTION('ref_axis',(0.,0.,-1.));
#4253=DIRECTION('center_axis',(0.,1.,0.));
#4254=DIRECTION('ref_axis',(1.,0.,0.));
#4255=DIRECTION('center_axis',(0.,1.,0.));
#4256=DIRECTION('ref_axis',(1.,0.,0.));
#4257=DIRECTION('center_axis',(0.,1.,0.));
#4258=DIRECTION('ref_axis',(0.,0.,1.));
#4259=DIRECTION('center_axis',(0.,-1.,0.));
#4260=DIRECTION('ref_axis',(1.,0.,0.));
#4261=DIRECTION('center_axis',(0.,-1.,0.));
#4262=DIRECTION('ref_axis',(1.,0.,0.));
#4263=DIRECTION('center_axis',(0.,-1.,0.));
#4264=DIRECTION('ref_axis',(1.,0.,0.));
#4265=DIRECTION('',(0.707106781186548,0.707106781186547,8.65956056235494E-17));
#4266=DIRECTION('center_axis',(0.,-1.,0.));
#4267=DIRECTION('ref_axis',(1.,0.,0.));
#4268=DIRECTION('center_axis',(0.,-1.,0.));
#4269=DIRECTION('ref_axis',(1.,0.,0.));
#4270=DIRECTION('',(0.,1.,0.));
#4271=DIRECTION('center_axis',(0.,1.,0.));
#4272=DIRECTION('ref_axis',(1.,0.,0.));
#4273=DIRECTION('center_axis',(0.,-1.,0.));
#4274=DIRECTION('ref_axis',(1.,0.,0.));
#4275=DIRECTION('',(-0.707106781186547,0.707106781186548,-8.65956056235493E-17));
#4276=DIRECTION('center_axis',(0.,-1.,0.));
#4277=DIRECTION('ref_axis',(0.,0.,-1.));
#4278=DIRECTION('center_axis',(0.,-1.,0.));
#4279=DIRECTION('ref_axis',(1.,0.,0.));
#4280=DIRECTION('center_axis',(0.,1.,0.));
#4281=DIRECTION('ref_axis',(1.,0.,0.));
#4282=DIRECTION('center_axis',(0.,1.,0.));
#4283=DIRECTION('ref_axis',(1.,0.,0.));
#4284=DIRECTION('',(-0.447213595499958,0.894427190999916,-5.47678698264203E-17));
#4285=DIRECTION('center_axis',(0.,-1.,0.));
#4286=DIRECTION('ref_axis',(1.,0.,0.));
#4287=DIRECTION('',(0.,1.,0.));
#4288=DIRECTION('axis',(0.,0.,1.));
#4289=DIRECTION('refdir',(1.,0.,0.));
#4290=DIRECTION('center_axis',(0.,1.,0.));
#4291=DIRECTION('ref_axis',(1.,0.,0.));
#4292=DIRECTION('center_axis',(0.,-1.,0.));
#4293=DIRECTION('ref_axis',(1.,0.,0.));
#4294=DIRECTION('',(0.,-1.,0.));
#4295=DIRECTION('center_axis',(0.,-1.,0.));
#4296=DIRECTION('ref_axis',(1.,0.,0.));
#4297=DIRECTION('center_axis',(0.,1.,0.));
#4298=DIRECTION('ref_axis',(1.,0.,0.));
#4299=DIRECTION('center_axis',(0.,1.,0.));
#4300=DIRECTION('ref_axis',(1.,0.,0.));
#4301=DIRECTION('',(0.,-1.,0.));
#4302=DIRECTION('center_axis',(0.,1.,0.));
#4303=DIRECTION('ref_axis',(1.,0.,0.));
#4304=DIRECTION('center_axis',(0.,1.,0.));
#4305=DIRECTION('ref_axis',(1.,0.,0.));
#4306=DIRECTION('center_axis',(0.,1.,0.));
#4307=DIRECTION('ref_axis',(1.,0.,0.));
#4308=DIRECTION('axis',(0.,0.,1.));
#4309=DIRECTION('refdir',(1.,0.,0.));
#4310=DIRECTION('center_axis',(0.,1.,0.));
#4311=DIRECTION('ref_axis',(1.,0.,0.));
#4312=DIRECTION('center_axis',(0.,-1.,0.));
#4313=DIRECTION('ref_axis',(1.,0.,0.));
#4314=DIRECTION('',(0.,-1.,0.));
#4315=DIRECTION('center_axis',(0.,-1.,0.));
#4316=DIRECTION('ref_axis',(1.,0.,0.));
#4317=DIRECTION('center_axis',(0.,1.,0.));
#4318=DIRECTION('ref_axis',(1.,0.,0.));
#4319=DIRECTION('center_axis',(0.,1.,0.));
#4320=DIRECTION('ref_axis',(1.,0.,0.));
#4321=DIRECTION('',(0.,-1.,0.));
#4322=DIRECTION('center_axis',(0.,1.,0.));
#4323=DIRECTION('ref_axis',(1.,0.,0.));
#4324=DIRECTION('center_axis',(0.,1.,0.));
#4325=DIRECTION('ref_axis',(1.,0.,0.));
#4326=DIRECTION('center_axis',(0.,1.,0.));
#4327=DIRECTION('ref_axis',(1.,0.,0.));
#4328=DIRECTION('axis',(0.,0.,1.));
#4329=DIRECTION('refdir',(1.,0.,0.));
#4330=DIRECTION('axis',(0.,0.,1.));
#4331=DIRECTION('refdir',(1.,0.,0.));
#4332=DIRECTION('center_axis',(0.,-1.,0.));
#4333=DIRECTION('ref_axis',(0.,0.,-1.));
#4334=DIRECTION('center_axis',(0.,-1.,0.));
#4335=DIRECTION('ref_axis',(1.,0.,0.));
#4336=DIRECTION('center_axis',(0.,-1.,0.));
#4337=DIRECTION('ref_axis',(1.,0.,0.));
#4338=DIRECTION('center_axis',(1.,0.,1.22464679914735E-16));
#4339=DIRECTION('ref_axis',(-1.22464679914735E-16,0.,1.));
#4340=DIRECTION('center_axis',(0.,1.,0.));
#4341=DIRECTION('ref_axis',(1.,0.,0.));
#4342=DIRECTION('center_axis',(0.,1.,0.));
#4343=DIRECTION('ref_axis',(1.,0.,0.));
#4344=DIRECTION('center_axis',(0.,-1.,0.));
#4345=DIRECTION('ref_axis',(1.,0.,0.));
#4346=DIRECTION('',(0.,1.,0.));
#4347=DIRECTION('center_axis',(0.,-1.,0.));
#4348=DIRECTION('ref_axis',(1.,0.,0.));
#4349=DIRECTION('center_axis',(0.,-1.,0.));
#4350=DIRECTION('ref_axis',(1.,0.,0.));
#4351=DIRECTION('center_axis',(0.,-1.,0.));
#4352=DIRECTION('ref_axis',(1.,0.,0.));
#4353=DIRECTION('',(0.,1.,0.));
#4354=DIRECTION('center_axis',(0.,-1.,0.));
#4355=DIRECTION('ref_axis',(1.,0.,0.));
#4356=DIRECTION('center_axis',(0.,1.,0.));
#4357=DIRECTION('ref_axis',(1.,0.,0.));
#4358=DIRECTION('',(-0.707106781186547,0.707106781186548,-8.65956056235493E-17));
#4359=DIRECTION('center_axis',(0.,-1.,0.));
#4360=DIRECTION('ref_axis',(1.,0.,0.));
#4361=DIRECTION('center_axis',(0.,1.,0.));
#4362=DIRECTION('ref_axis',(0.,0.,1.));
#4363=DIRECTION('center_axis',(0.,-1.,0.));
#4364=DIRECTION('ref_axis',(1.,0.,0.));
#4365=DIRECTION('center_axis',(0.,-1.,0.));
#4366=DIRECTION('ref_axis',(1.,0.,0.));
#4367=DIRECTION('',(0.,1.,0.));
#4368=DIRECTION('center_axis',(0.,-1.,0.));
#4369=DIRECTION('ref_axis',(0.,0.,-1.));
#4370=DIRECTION('center_axis',(0.,-1.,0.));
#4371=DIRECTION('ref_axis',(1.,0.,0.));
#4372=DIRECTION('center_axis',(0.,-1.,0.));
#4373=DIRECTION('ref_axis',(1.,0.,0.));
#4374=DIRECTION('',(0.707106781186547,0.707106781186548,8.65956056235493E-17));
#4375=DIRECTION('axis',(0.,0.,1.));
#4376=DIRECTION('refdir',(1.,0.,0.));
#4377=DIRECTION('center_axis',(0.,-1.,0.));
#4378=DIRECTION('ref_axis',(0.,0.,-1.));
#4379=DIRECTION('center_axis',(0.,-1.,0.));
#4380=DIRECTION('ref_axis',(1.,0.,0.));
#4381=DIRECTION('center_axis',(0.,-1.,0.));
#4382=DIRECTION('ref_axis',(1.,0.,0.));
#4383=DIRECTION('center_axis',(1.,0.,1.22464679914735E-16));
#4384=DIRECTION('ref_axis',(-1.22464679914735E-16,0.,1.));
#4385=DIRECTION('center_axis',(0.,1.,0.));
#4386=DIRECTION('ref_axis',(1.,0.,0.));
#4387=DIRECTION('center_axis',(0.,1.,0.));
#4388=DIRECTION('ref_axis',(1.,0.,0.));
#4389=DIRECTION('center_axis',(0.,-1.,0.));
#4390=DIRECTION('ref_axis',(1.,0.,0.));
#4391=DIRECTION('center_axis',(0.,-1.,0.));
#4392=DIRECTION('ref_axis',(1.,0.,0.));
#4393=DIRECTION('',(0.,1.,0.));
#4394=DIRECTION('center_axis',(0.,1.,0.));
#4395=DIRECTION('ref_axis',(0.,0.,1.));
#4396=DIRECTION('center_axis',(0.,-1.,0.));
#4397=DIRECTION('ref_axis',(1.,0.,0.));
#4398=DIRECTION('center_axis',(0.,-1.,0.));
#4399=DIRECTION('ref_axis',(1.,0.,0.));
#4400=DIRECTION('center_axis',(0.,-1.,0.));
#4401=DIRECTION('ref_axis',(1.,0.,0.));
#4402=DIRECTION('center_axis',(0.,-1.,0.));
#4403=DIRECTION('ref_axis',(1.,0.,0.));
#4404=DIRECTION('',(0.707106781186548,0.707106781186547,8.65956056235494E-17));
#4405=DIRECTION('center_axis',(0.,-1.,0.));
#4406=DIRECTION('ref_axis',(1.,0.,0.));
#4407=DIRECTION('center_axis',(0.,-1.,0.));
#4408=DIRECTION('ref_axis',(1.,0.,0.));
#4409=DIRECTION('',(0.,1.,0.));
#4410=DIRECTION('center_axis',(0.,1.,0.));
#4411=DIRECTION('ref_axis',(1.,0.,0.));
#4412=DIRECTION('center_axis',(0.,-1.,0.));
#4413=DIRECTION('ref_axis',(1.,0.,0.));
#4414=DIRECTION('',(-0.707106781186548,0.707106781186547,-8.65956056235494E-17));
#4415=DIRECTION('center_axis',(0.,-1.,0.));
#4416=DIRECTION('ref_axis',(0.,0.,-1.));
#4417=DIRECTION('center_axis',(0.,-1.,0.));
#4418=DIRECTION('ref_axis',(1.,0.,0.));
#4419=DIRECTION('',(0.,1.,0.));
#4420=DIRECTION('axis',(0.,0.,1.));
#4421=DIRECTION('refdir',(1.,0.,0.));
#4422=DIRECTION('center_axis',(0.,0.,1.));
#4423=DIRECTION('ref_axis',(1.,0.,0.));
#4424=DIRECTION('center_axis',(1.22464679914735E-16,-1.,0.));
#4425=DIRECTION('ref_axis',(-1.,-1.22464679914735E-16,0.));
#4426=DIRECTION('center_axis',(0.707106781186548,0.,0.707106781186548));
#4427=DIRECTION('ref_axis',(0.707106781186548,0.,-0.707106781186548));
#4428=DIRECTION('center_axis',(8.65956056235494E-17,-1.,-8.65956056235493E-17));
#4429=DIRECTION('ref_axis',(-0.707106781186547,-1.22464679914735E-16,0.707106781186547));
#4430=DIRECTION('center_axis',(1.,0.,0.));
#4431=DIRECTION('ref_axis',(6.12323399573676E-17,0.,-1.));
#4432=DIRECTION('center_axis',(7.49879891330929E-33,-1.,-1.22464679914735E-16));
#4433=DIRECTION('ref_axis',(-6.12323399573676E-17,-1.22464679914735E-16,
1.));
#4434=DIRECTION('center_axis',(0.707106781186548,0.,-0.707106781186548));
#4435=DIRECTION('ref_axis',(-0.707106781186548,0.,-0.707106781186548));
#4436=DIRECTION('center_axis',(-8.65956056235493E-17,-1.,-8.65956056235494E-17));
#4437=DIRECTION('ref_axis',(0.707106781186547,-1.22464679914735E-16,0.707106781186547));
#4438=DIRECTION('center_axis',(0.,0.,-1.));
#4439=DIRECTION('ref_axis',(-1.,0.,-1.22464679914735E-16));
#4440=DIRECTION('center_axis',(-1.22464679914735E-16,-1.,-1.49975978266186E-32));
#4441=DIRECTION('ref_axis',(1.,-1.22464679914735E-16,1.22464679914735E-16));
#4442=DIRECTION('center_axis',(-0.707106781186547,0.,-0.707106781186548));
#4443=DIRECTION('ref_axis',(-0.707106781186548,0.,0.707106781186547));
#4444=DIRECTION('center_axis',(-8.65956056235493E-17,-1.,8.65956056235493E-17));
#4445=DIRECTION('ref_axis',(0.707106781186548,-1.22464679914735E-16,-0.707106781186547));
#4446=DIRECTION('center_axis',(-1.,0.,0.));
#4447=DIRECTION('ref_axis',(-1.83697019872103E-16,0.,1.));
#4448=DIRECTION('center_axis',(-2.24963967399279E-32,-1.,1.22464679914735E-16));
#4449=DIRECTION('ref_axis',(1.83697019872103E-16,-1.22464679914735E-16,
-1.));
#4450=DIRECTION('center_axis',(-0.707106781186548,0.,0.707106781186548));
#4451=DIRECTION('ref_axis',(0.707106781186547,0.,0.707106781186548));
#4452=DIRECTION('center_axis',(8.65956056235493E-17,-1.,8.65956056235493E-17));
#4453=DIRECTION('ref_axis',(-0.707106781186547,-1.22464679914735E-16,-0.707106781186548));
#4454=DIRECTION('axis',(0.,0.,1.));
#4455=DIRECTION('refdir',(1.,0.,0.));
#4456=DIRECTION('center_axis',(0.,0.,1.));
#4457=DIRECTION('ref_axis',(1.,0.,0.));
#4458=DIRECTION('center_axis',(0.,-1.,0.));
#4459=DIRECTION('ref_axis',(0.,0.,-1.));
#4460=DIRECTION('center_axis',(0.,-1.,0.));
#4461=DIRECTION('ref_axis',(0.,0.,-1.));
#4462=DIRECTION('center_axis',(0.,1.,0.));
#4463=DIRECTION('ref_axis',(1.,0.,0.));
#4464=DIRECTION('center_axis',(0.,1.,0.));
#4465=DIRECTION('ref_axis',(1.,0.,0.));
#4466=DIRECTION('center_axis',(0.,1.,0.));
#4467=DIRECTION('ref_axis',(1.,0.,0.));
#4468=DIRECTION('center_axis',(0.,1.,0.));
#4469=DIRECTION('ref_axis',(1.,0.,0.));
#4470=DIRECTION('',(0.,-1.,0.));
#4471=DIRECTION('center_axis',(0.,-1.,0.));
#4472=DIRECTION('ref_axis',(1.,0.,0.));
#4473=DIRECTION('center_axis',(0.,1.,0.));
#4474=DIRECTION('ref_axis',(1.,0.,0.));
#4475=DIRECTION('center_axis',(0.,1.,0.));
#4476=DIRECTION('ref_axis',(1.,0.,0.));
#4477=DIRECTION('center_axis',(0.,1.,0.));
#4478=DIRECTION('ref_axis',(1.,0.,0.));
#4479=DIRECTION('center_axis',(0.,1.,0.));
#4480=DIRECTION('ref_axis',(1.,0.,0.));
#4481=DIRECTION('center_axis',(0.,1.,0.));
#4482=DIRECTION('ref_axis',(1.,0.,0.));
#4483=DIRECTION('center_axis',(0.,1.,0.));
#4484=DIRECTION('ref_axis',(1.,0.,0.));
#4485=DIRECTION('center_axis',(0.,-1.,0.));
#4486=DIRECTION('ref_axis',(1.,0.,0.));
#4487=DIRECTION('center_axis',(0.,-1.,0.));
#4488=DIRECTION('ref_axis',(0.,0.,-1.));
#4489=DIRECTION('center_axis',(6.12323399573677E-17,0.,1.));
#4490=DIRECTION('ref_axis',(1.,0.,0.));
#4491=DIRECTION('center_axis',(0.,-1.,0.));
#4492=DIRECTION('ref_axis',(0.,0.,-1.));
#4493=DIRECTION('center_axis',(0.,1.,0.));
#4494=DIRECTION('ref_axis',(1.,0.,0.));
#4495=DIRECTION('center_axis',(0.,-1.,0.));
#4496=DIRECTION('ref_axis',(1.,0.,0.));
#4497=DIRECTION('center_axis',(0.,-1.,0.));
#4498=DIRECTION('ref_axis',(0.,0.,-1.));
#4499=DIRECTION('center_axis',(0.,0.,1.));
#4500=DIRECTION('ref_axis',(1.,0.,0.));
#4501=DIRECTION('center_axis',(0.,-1.,0.));
#4502=DIRECTION('ref_axis',(0.,0.,-1.));
#4503=DIRECTION('center_axis',(0.,1.,0.));
#4504=DIRECTION('ref_axis',(1.,0.,0.));
#4505=DIRECTION('center_axis',(0.,-1.,0.));
#4506=DIRECTION('ref_axis',(1.,0.,0.));
#4507=DIRECTION('center_axis',(0.,-1.,0.));
#4508=DIRECTION('ref_axis',(0.,0.,-1.));
#4509=DIRECTION('center_axis',(0.,0.,1.));
#4510=DIRECTION('ref_axis',(1.,0.,0.));
#4511=DIRECTION('center_axis',(0.,-1.,0.));
#4512=DIRECTION('ref_axis',(0.,0.,-1.));
#4513=DIRECTION('center_axis',(0.,1.,0.));
#4514=DIRECTION('ref_axis',(1.,0.,0.));
#4515=DIRECTION('center_axis',(0.,-1.,0.));
#4516=DIRECTION('ref_axis',(1.,0.,0.));
#4517=DIRECTION('center_axis',(0.,-1.,0.));
#4518=DIRECTION('ref_axis',(0.,0.,-1.));
#4519=DIRECTION('center_axis',(0.,0.,1.));
#4520=DIRECTION('ref_axis',(1.,0.,0.));
#4521=DIRECTION('center_axis',(0.,-1.,0.));
#4522=DIRECTION('ref_axis',(0.,0.,-1.));
#4523=DIRECTION('center_axis',(0.,1.,0.));
#4524=DIRECTION('ref_axis',(1.,0.,0.));
#4525=DIRECTION('center_axis',(0.,-1.,0.));
#4526=DIRECTION('ref_axis',(1.,0.,0.));
#4527=DIRECTION('center_axis',(0.,-1.,0.));
#4528=DIRECTION('ref_axis',(0.,0.,-1.));
#4529=DIRECTION('center_axis',(6.12323399573676E-17,0.,1.));
#4530=DIRECTION('ref_axis',(1.,0.,0.));
#4531=DIRECTION('center_axis',(0.,-1.,0.));
#4532=DIRECTION('ref_axis',(0.,0.,-1.));
#4533=DIRECTION('center_axis',(0.,1.,0.));
#4534=DIRECTION('ref_axis',(1.,0.,0.));
#4535=DIRECTION('center_axis',(0.,-1.,0.));
#4536=DIRECTION('ref_axis',(1.,0.,0.));
#4537=DIRECTION('center_axis',(0.,-1.,0.));
#4538=DIRECTION('ref_axis',(0.,0.,-1.));
#4539=DIRECTION('center_axis',(0.,0.,1.));
#4540=DIRECTION('ref_axis',(1.,0.,0.));
#4541=DIRECTION('center_axis',(0.,-1.,0.));
#4542=DIRECTION('ref_axis',(0.,0.,-1.));
#4543=DIRECTION('center_axis',(0.,1.,0.));
#4544=DIRECTION('ref_axis',(1.,0.,0.));
#4545=DIRECTION('center_axis',(0.,1.,0.));
#4546=DIRECTION('ref_axis',(1.,0.,0.));
#4547=DIRECTION('',(0.,1.,0.));
#4548=DIRECTION('center_axis',(0.,-1.,0.));
#4549=DIRECTION('ref_axis',(1.,0.,0.));
#4550=DIRECTION('center_axis',(0.,-1.,0.));
#4551=DIRECTION('ref_axis',(1.,0.,0.));
#4552=DIRECTION('center_axis',(0.,1.,0.));
#4553=DIRECTION('ref_axis',(1.,0.,0.));
#4554=DIRECTION('center_axis',(0.,-1.,0.));
#4555=DIRECTION('ref_axis',(0.,0.,-1.));
#4556=DIRECTION('center_axis',(0.,0.,1.));
#4557=DIRECTION('ref_axis',(1.,0.,0.));
#4558=DIRECTION('center_axis',(0.,-1.,0.));
#4559=DIRECTION('ref_axis',(0.,0.,-1.));
#4560=DIRECTION('center_axis',(0.,-1.,0.));
#4561=DIRECTION('ref_axis',(-1.,0.,0.));
#4562=DIRECTION('center_axis',(0.,1.,0.));
#4563=DIRECTION('ref_axis',(1.,0.,0.));
#4564=DIRECTION('axis',(0.,0.,1.));
#4565=DIRECTION('refdir',(1.,0.,0.));
#4566=DIRECTION('center_axis',(0.,1.,0.));
#4567=DIRECTION('ref_axis',(0.,0.,1.));
#4568=DIRECTION('center_axis',(0.,-1.,0.));
#4569=DIRECTION('ref_axis',(1.,0.,0.));
#4570=DIRECTION('center_axis',(0.,-1.,0.));
#4571=DIRECTION('ref_axis',(1.,0.,0.));
#4572=DIRECTION('center_axis',(0.,-1.,0.));
#4573=DIRECTION('ref_axis',(1.,0.,0.));
#4574=DIRECTION('center_axis',(0.,-1.,0.));
#4575=DIRECTION('ref_axis',(1.,0.,0.));
#4576=DIRECTION('',(0.,1.,0.));
#4577=DIRECTION('center_axis',(0.,-1.,0.));
#4578=DIRECTION('ref_axis',(0.,0.,-1.));
#4579=DIRECTION('center_axis',(0.,-1.,0.));
#4580=DIRECTION('ref_axis',(1.,0.,0.));
#4581=DIRECTION('center_axis',(0.,-1.,0.));
#4582=DIRECTION('ref_axis',(1.,0.,0.));
#4583=DIRECTION('',(0.,1.,0.));
#4584=DIRECTION('center_axis',(0.,1.,0.));
#4585=DIRECTION('ref_axis',(0.,0.,1.));
#4586=DIRECTION('center_axis',(0.,-1.,0.));
#4587=DIRECTION('ref_axis',(1.,0.,0.));
#4588=DIRECTION('center_axis',(0.,-1.,0.));
#4589=DIRECTION('ref_axis',(1.,0.,0.));
#4590=DIRECTION('center_axis',(0.,-1.,0.));
#4591=DIRECTION('ref_axis',(1.,0.,0.));
#4592=DIRECTION('center_axis',(0.,-1.,0.));
#4593=DIRECTION('ref_axis',(1.,0.,0.));
#4594=DIRECTION('',(0.,1.,0.));
#4595=DIRECTION('center_axis',(0.,-1.,0.));
#4596=DIRECTION('ref_axis',(0.,0.,-1.));
#4597=DIRECTION('center_axis',(0.,-1.,0.));
#4598=DIRECTION('ref_axis',(1.,0.,0.));
#4599=DIRECTION('center_axis',(0.,-1.,0.));
#4600=DIRECTION('ref_axis',(1.,0.,0.));
#4601=DIRECTION('',(0.,1.,0.));
#4602=DIRECTION('',(0.,0.,1.));
#4603=DIRECTION('',(1.,0.,0.));
#4604=DIRECTION('',(0.,0.,1.));
#4605=DIRECTION('',(1.,0.,0.));
#4606=DIRECTION('',(0.,0.,1.));
#4607=DIRECTION('',(1.,0.,0.));
#4608=DIRECTION('',(0.,0.,1.));
#4609=DIRECTION('',(1.,0.,0.));
#4610=DIRECTION('',(0.,0.,1.));
#4611=DIRECTION('',(1.,0.,0.));
#4612=DIRECTION('axis',(0.,0.,1.));
#4613=DIRECTION('refdir',(1.,0.,0.));
#4614=DIRECTION('axis',(0.,0.,1.));
#4615=DIRECTION('refdir',(1.,0.,0.));
#4616=DIRECTION('center_axis',(0.,1.,0.));
#4617=DIRECTION('ref_axis',(1.,0.,0.));
#4618=DIRECTION('center_axis',(0.,1.,0.));
#4619=DIRECTION('ref_axis',(1.,0.,0.));
#4620=DIRECTION('',(0.,1.,0.));
#4621=DIRECTION('center_axis',(0.,-1.,0.));
#4622=DIRECTION('ref_axis',(1.,0.,0.));
#4623=DIRECTION('center_axis',(0.,1.,0.));
#4624=DIRECTION('ref_axis',(1.,0.,0.));
#4625=DIRECTION('center_axis',(0.,1.,0.));
#4626=DIRECTION('ref_axis',(1.,0.,0.));
#4627=DIRECTION('',(0.,1.,0.));
#4628=DIRECTION('center_axis',(0.,-1.,0.));
#4629=DIRECTION('ref_axis',(1.,0.,0.));
#4630=DIRECTION('center_axis',(0.,1.,0.));
#4631=DIRECTION('ref_axis',(1.,0.,0.));
#4632=DIRECTION('center_axis',(0.,1.,0.));
#4633=DIRECTION('ref_axis',(1.,0.,0.));
#4634=DIRECTION('',(0.,1.,0.));
#4635=DIRECTION('center_axis',(0.,-1.,0.));
#4636=DIRECTION('ref_axis',(1.,0.,0.));
#4637=DIRECTION('center_axis',(0.,1.,0.));
#4638=DIRECTION('ref_axis',(1.,0.,0.));
#4639=DIRECTION('center_axis',(0.,1.,0.));
#4640=DIRECTION('ref_axis',(1.,0.,0.));
#4641=DIRECTION('',(0.,1.,0.));
#4642=DIRECTION('center_axis',(0.,-1.,0.));
#4643=DIRECTION('ref_axis',(1.,0.,0.));
#4644=DIRECTION('center_axis',(0.,1.,0.));
#4645=DIRECTION('ref_axis',(1.,0.,0.));
#4646=DIRECTION('center_axis',(0.,-1.,0.));
#4647=DIRECTION('ref_axis',(1.,0.,0.));
#4648=DIRECTION('',(0.,-1.,0.));
#4649=DIRECTION('center_axis',(0.,-1.,0.));
#4650=DIRECTION('ref_axis',(1.,0.,0.));
#4651=DIRECTION('center_axis',(0.,1.,0.));
#4652=DIRECTION('ref_axis',(1.,0.,0.));
#4653=DIRECTION('center_axis',(0.,1.,0.));
#4654=DIRECTION('ref_axis',(1.,0.,0.));
#4655=DIRECTION('center_axis',(0.,1.,0.));
#4656=DIRECTION('ref_axis',(1.,0.,0.));
#4657=DIRECTION('',(0.,-1.,0.));
#4658=DIRECTION('center_axis',(0.,-1.,0.));
#4659=DIRECTION('ref_axis',(1.,0.,0.));
#4660=DIRECTION('center_axis',(0.,1.,0.));
#4661=DIRECTION('ref_axis',(1.,0.,0.));
#4662=DIRECTION('center_axis',(0.,1.,0.));
#4663=DIRECTION('ref_axis',(1.,0.,0.));
#4664=DIRECTION('',(0.,-1.,0.));
#4665=DIRECTION('center_axis',(0.,1.,0.));
#4666=DIRECTION('ref_axis',(1.,0.,0.));
#4667=DIRECTION('center_axis',(0.,1.,0.));
#4668=DIRECTION('ref_axis',(1.,0.,0.));
#4669=DIRECTION('center_axis',(0.,1.,0.));
#4670=DIRECTION('ref_axis',(1.,0.,0.));
#4671=DIRECTION('axis',(0.,0.,1.));
#4672=DIRECTION('refdir',(1.,0.,0.));
#4673=DIRECTION('center_axis',(0.,1.,0.));
#4674=DIRECTION('ref_axis',(1.,0.,0.));
#4675=DIRECTION('center_axis',(0.,1.,0.));
#4676=DIRECTION('ref_axis',(1.,0.,0.));
#4677=DIRECTION('',(0.,1.,0.));
#4678=DIRECTION('center_axis',(0.,-1.,0.));
#4679=DIRECTION('ref_axis',(1.,0.,0.));
#4680=DIRECTION('center_axis',(0.,1.,0.));
#4681=DIRECTION('ref_axis',(1.,0.,0.));
#4682=DIRECTION('center_axis',(0.,1.,0.));
#4683=DIRECTION('ref_axis',(1.,0.,0.));
#4684=DIRECTION('',(0.,1.,0.));
#4685=DIRECTION('center_axis',(0.,-1.,0.));
#4686=DIRECTION('ref_axis',(1.,0.,0.));
#4687=DIRECTION('center_axis',(0.,1.,0.));
#4688=DIRECTION('ref_axis',(1.,0.,0.));
#4689=DIRECTION('center_axis',(0.,1.,0.));
#4690=DIRECTION('ref_axis',(1.,0.,0.));
#4691=DIRECTION('',(0.,1.,0.));
#4692=DIRECTION('center_axis',(0.,-1.,0.));
#4693=DIRECTION('ref_axis',(1.,0.,0.));
#4694=DIRECTION('center_axis',(0.,1.,0.));
#4695=DIRECTION('ref_axis',(1.,0.,0.));
#4696=DIRECTION('center_axis',(0.,1.,0.));
#4697=DIRECTION('ref_axis',(1.,0.,0.));
#4698=DIRECTION('',(0.,1.,0.));
#4699=DIRECTION('center_axis',(0.,-1.,0.));
#4700=DIRECTION('ref_axis',(1.,0.,0.));
#4701=DIRECTION('center_axis',(0.,1.,0.));
#4702=DIRECTION('ref_axis',(1.,0.,0.));
#4703=DIRECTION('center_axis',(0.,-1.,0.));
#4704=DIRECTION('ref_axis',(1.,0.,0.));
#4705=DIRECTION('',(0.,-1.,0.));
#4706=DIRECTION('center_axis',(0.,-1.,0.));
#4707=DIRECTION('ref_axis',(1.,0.,0.));
#4708=DIRECTION('center_axis',(0.,1.,0.));
#4709=DIRECTION('ref_axis',(1.,0.,0.));
#4710=DIRECTION('center_axis',(0.,-1.,0.));
#4711=DIRECTION('ref_axis',(1.,0.,0.));
#4712=DIRECTION('center_axis',(0.,1.,0.));
#4713=DIRECTION('ref_axis',(1.,0.,0.));
#4714=DIRECTION('center_axis',(0.,-1.,0.));
#4715=DIRECTION('ref_axis',(1.,0.,0.));
#4716=DIRECTION('',(0.,-1.,0.));
#4717=DIRECTION('center_axis',(0.,1.,0.));
#4718=DIRECTION('ref_axis',(1.,0.,0.));
#4719=DIRECTION('center_axis',(0.,1.,0.));
#4720=DIRECTION('ref_axis',(1.,0.,0.));
#4721=DIRECTION('',(0.,-1.,0.));
#4722=DIRECTION('center_axis',(0.,1.,0.));
#4723=DIRECTION('ref_axis',(1.,0.,0.));
#4724=DIRECTION('center_axis',(0.,1.,0.));
#4725=DIRECTION('ref_axis',(1.,0.,0.));
#4726=DIRECTION('center_axis',(0.,1.,0.));
#4727=DIRECTION('ref_axis',(1.,0.,0.));
#4728=DIRECTION('axis',(0.,0.,1.));
#4729=DIRECTION('refdir',(1.,0.,0.));
#4730=DIRECTION('center_axis',(0.,1.,0.));
#4731=DIRECTION('ref_axis',(1.,0.,0.));
#4732=DIRECTION('center_axis',(0.,-1.,0.));
#4733=DIRECTION('ref_axis',(1.,0.,0.));
#4734=DIRECTION('',(0.,-1.,0.));
#4735=DIRECTION('center_axis',(0.,-1.,0.));
#4736=DIRECTION('ref_axis',(1.,0.,0.));
#4737=DIRECTION('center_axis',(0.,1.,0.));
#4738=DIRECTION('ref_axis',(1.,0.,0.));
#4739=DIRECTION('center_axis',(0.,1.,0.));
#4740=DIRECTION('ref_axis',(1.,0.,0.));
#4741=DIRECTION('',(0.,-1.,0.));
#4742=DIRECTION('center_axis',(0.,1.,0.));
#4743=DIRECTION('ref_axis',(1.,0.,0.));
#4744=DIRECTION('center_axis',(0.,1.,0.));
#4745=DIRECTION('ref_axis',(1.,0.,0.));
#4746=DIRECTION('center_axis',(0.,1.,0.));
#4747=DIRECTION('ref_axis',(1.,0.,0.));
#4748=DIRECTION('axis',(0.,0.,1.));
#4749=DIRECTION('refdir',(1.,0.,0.));
#4750=DIRECTION('center_axis',(0.,1.,0.));
#4751=DIRECTION('ref_axis',(1.,0.,0.));
#4752=DIRECTION('center_axis',(0.,1.,0.));
#4753=DIRECTION('ref_axis',(1.,0.,0.));
#4754=DIRECTION('',(0.,1.,0.));
#4755=DIRECTION('center_axis',(0.,-1.,0.));
#4756=DIRECTION('ref_axis',(1.,0.,0.));
#4757=DIRECTION('center_axis',(0.,1.,0.));
#4758=DIRECTION('ref_axis',(1.,0.,0.));
#4759=DIRECTION('center_axis',(0.,1.,0.));
#4760=DIRECTION('ref_axis',(1.,0.,0.));
#4761=DIRECTION('',(0.,1.,0.));
#4762=DIRECTION('center_axis',(0.,-1.,0.));
#4763=DIRECTION('ref_axis',(1.,0.,0.));
#4764=DIRECTION('center_axis',(0.,1.,0.));
#4765=DIRECTION('ref_axis',(1.,0.,0.));
#4766=DIRECTION('center_axis',(0.,1.,0.));
#4767=DIRECTION('ref_axis',(1.,0.,0.));
#4768=DIRECTION('',(0.,1.,0.));
#4769=DIRECTION('center_axis',(0.,-1.,0.));
#4770=DIRECTION('ref_axis',(1.,0.,0.));
#4771=DIRECTION('center_axis',(0.,1.,0.));
#4772=DIRECTION('ref_axis',(1.,0.,0.));
#4773=DIRECTION('center_axis',(0.,1.,0.));
#4774=DIRECTION('ref_axis',(1.,0.,0.));
#4775=DIRECTION('',(0.,1.,0.));
#4776=DIRECTION('center_axis',(0.,-1.,0.));
#4777=DIRECTION('ref_axis',(1.,0.,0.));
#4778=DIRECTION('center_axis',(0.,1.,0.));
#4779=DIRECTION('ref_axis',(1.,0.,0.));
#4780=DIRECTION('center_axis',(0.,-1.,0.));
#4781=DIRECTION('ref_axis',(1.,0.,0.));
#4782=DIRECTION('',(0.,-1.,0.));
#4783=DIRECTION('center_axis',(0.,-1.,0.));
#4784=DIRECTION('ref_axis',(1.,0.,0.));
#4785=DIRECTION('center_axis',(0.,1.,0.));
#4786=DIRECTION('ref_axis',(1.,0.,0.));
#4787=DIRECTION('center_axis',(0.,1.,0.));
#4788=DIRECTION('ref_axis',(1.,0.,0.));
#4789=DIRECTION('',(0.,-1.,0.));
#4790=DIRECTION('center_axis',(0.,1.,0.));
#4791=DIRECTION('ref_axis',(1.,0.,0.));
#4792=DIRECTION('center_axis',(0.,1.,0.));
#4793=DIRECTION('ref_axis',(1.,0.,0.));
#4794=DIRECTION('center_axis',(0.,1.,0.));
#4795=DIRECTION('ref_axis',(1.,0.,0.));
#4796=DIRECTION('axis',(0.,0.,1.));
#4797=DIRECTION('refdir',(1.,0.,0.));
#4798=DIRECTION('center_axis',(0.,1.,0.));
#4799=DIRECTION('ref_axis',(0.,0.,1.));
#4800=DIRECTION('center_axis',(0.,-1.,0.));
#4801=DIRECTION('ref_axis',(1.,0.,0.));
#4802=DIRECTION('center_axis',(0.,-1.,0.));
#4803=DIRECTION('ref_axis',(1.,0.,0.));
#4804=DIRECTION('center_axis',(0.,-1.,0.));
#4805=DIRECTION('ref_axis',(1.,0.,0.));
#4806=DIRECTION('',(0.707106781186547,0.707106781186548,8.65956056235493E-17));
#4807=DIRECTION('center_axis',(0.,-1.,0.));
#4808=DIRECTION('ref_axis',(1.,0.,0.));
#4809=DIRECTION('center_axis',(0.,-1.,0.));
#4810=DIRECTION('ref_axis',(1.,0.,0.));
#4811=DIRECTION('',(0.,1.,0.));
#4812=DIRECTION('center_axis',(0.,1.,0.));
#4813=DIRECTION('ref_axis',(1.,0.,0.));
#4814=DIRECTION('center_axis',(0.,-1.,0.));
#4815=DIRECTION('ref_axis',(1.,0.,0.));
#4816=DIRECTION('',(-0.707106781186547,0.707106781186548,-8.65956056235493E-17));
#4817=DIRECTION('center_axis',(0.,-1.,0.));
#4818=DIRECTION('ref_axis',(0.,0.,-1.));
#4819=DIRECTION('center_axis',(0.,-1.,0.));
#4820=DIRECTION('ref_axis',(1.,0.,0.));
#4821=DIRECTION('center_axis',(0.,1.,0.));
#4822=DIRECTION('ref_axis',(1.,0.,0.));
#4823=DIRECTION('center_axis',(0.,1.,0.));
#4824=DIRECTION('ref_axis',(1.,0.,0.));
#4825=DIRECTION('',(-0.447213595499958,0.894427190999916,-5.47678698264203E-17));
#4826=DIRECTION('center_axis',(0.,-1.,0.));
#4827=DIRECTION('ref_axis',(1.,0.,0.));
#4828=DIRECTION('center_axis',(0.,1.,0.));
#4829=DIRECTION('ref_axis',(1.,0.,0.));
#4830=DIRECTION('',(0.,1.,0.));
#4831=DIRECTION('center_axis',(0.,1.,0.));
#4832=DIRECTION('ref_axis',(1.,0.,0.));
#4833=DIRECTION('center_axis',(0.,-1.,0.));
#4834=DIRECTION('ref_axis',(1.,0.,0.));
#4835=DIRECTION('',(-0.707106781186547,0.707106781186548,-8.65956056235493E-17));
#4836=DIRECTION('center_axis',(0.,-1.,0.));
#4837=DIRECTION('ref_axis',(0.,0.,-1.));
#4838=DIRECTION('center_axis',(0.866025403784439,0.,-0.5));
#4839=DIRECTION('ref_axis',(0.5,0.,0.866025403784439));
#4840=DIRECTION('',(-0.5,0.,-0.866025403784439));
#4841=DIRECTION('',(0.,-1.,0.));
#4842=DIRECTION('',(0.5,0.,0.866025403784439));
#4843=DIRECTION('',(0.,-1.,0.));
#4844=DIRECTION('center_axis',(1.60246890531964E-16,0.,-1.));
#4845=DIRECTION('ref_axis',(1.,0.,1.60246890531964E-16));
#4846=DIRECTION('',(-1.,0.,-1.60246890531964E-16));
#4847=DIRECTION('',(0.,-1.,0.));
#4848=DIRECTION('',(1.,0.,1.60246890531964E-16));
#4849=DIRECTION('center_axis',(-0.866025403784439,0.,-0.5));
#4850=DIRECTION('ref_axis',(0.5,0.,-0.866025403784439));
#4851=DIRECTION('',(-0.5,0.,0.866025403784439));
#4852=DIRECTION('',(0.,-1.,0.));
#4853=DIRECTION('',(0.5,0.,-0.866025403784439));
#4854=DIRECTION('center_axis',(-0.866025403784439,0.,0.5));
#4855=DIRECTION('ref_axis',(-0.5,0.,-0.866025403784439));
#4856=DIRECTION('',(0.5,0.,0.866025403784439));
#4857=DIRECTION('',(0.,-1.,0.));
#4858=DIRECTION('',(-0.5,0.,-0.866025403784439));
#4859=DIRECTION('center_axis',(-1.60246890531964E-16,0.,1.));
#4860=DIRECTION('ref_axis',(-1.,0.,-1.60246890531964E-16));
#4861=DIRECTION('',(1.,0.,1.60246890531964E-16));
#4862=DIRECTION('',(0.,-1.,0.));
#4863=DIRECTION('',(-1.,0.,-1.60246890531964E-16));
#4864=DIRECTION('center_axis',(0.866025403784439,0.,0.5));
#4865=DIRECTION('ref_axis',(-0.5,0.,0.866025403784439));
#4866=DIRECTION('',(0.5,0.,-0.866025403784439));
#4867=DIRECTION('',(-0.5,0.,0.866025403784439));
#4868=DIRECTION('center_axis',(0.,1.,0.));
#4869=DIRECTION('ref_axis',(1.,0.,0.));
#4870=DIRECTION('center_axis',(0.,-1.,0.));
#4871=DIRECTION('ref_axis',(0.,0.,-1.));
#4872=DIRECTION('',(0.,0.,1.));
#4873=DIRECTION('',(1.,0.,0.));
#4874=DIRECTION('',(0.,0.,1.));
#4875=DIRECTION('',(1.,0.,0.));
#4876=DIRECTION('',(0.,0.,1.));
#4877=DIRECTION('',(1.,0.,0.));
#4878=DIRECTION('',(0.,0.,1.));
#4879=DIRECTION('',(1.,0.,0.));
#4880=DIRECTION('',(0.,0.,1.));
#4881=DIRECTION('',(1.,0.,0.));
#4882=DIRECTION('',(0.,0.,1.));
#4883=DIRECTION('',(1.,0.,0.));
#4884=DIRECTION('',(0.,0.,1.));
#4885=DIRECTION('',(1.,0.,0.));
#4886=DIRECTION('',(0.,0.,1.));
#4887=DIRECTION('',(1.,0.,0.));
#4888=DIRECTION('',(0.,-1.,2.22044604925031E-16));
#4889=DIRECTION('',(1.,0.,0.));
#4890=DIRECTION('',(0.,-1.,2.22044604925031E-16));
#4891=DIRECTION('',(1.,0.,0.));
#4892=DIRECTION('',(0.,-1.,2.22044604925031E-16));
#4893=DIRECTION('',(1.,0.,0.));
#4894=DIRECTION('',(0.,-1.,2.22044604925031E-16));
#4895=DIRECTION('',(1.,0.,0.));
#4896=DIRECTION('',(0.,-1.,2.22044604925031E-16));
#4897=DIRECTION('',(1.,0.,0.));
#4898=DIRECTION('',(0.,-1.,2.22044604925031E-16));
#4899=DIRECTION('',(1.,0.,0.));
#4900=DIRECTION('',(0.,-1.,2.22044604925031E-16));
#4901=DIRECTION('',(1.,0.,0.));
#4902=DIRECTION('',(0.,-1.,2.22044604925031E-16));
#4903=DIRECTION('',(1.,0.,0.));
#4904=DIRECTION('',(0.,0.,1.));
#4905=DIRECTION('',(1.,0.,0.));
#4906=DIRECTION('',(0.,0.,1.));
#4907=DIRECTION('',(1.,0.,0.));
#4908=DIRECTION('',(0.,0.,1.));
#4909=DIRECTION('',(-1.,1.22464679914735E-16,0.));
#4910=DIRECTION('',(0.,0.,1.));
#4911=DIRECTION('',(1.,0.,0.));
#4912=DIRECTION('',(0.,0.,1.));
#4913=DIRECTION('',(1.,0.,0.));
#4914=DIRECTION('',(0.,0.,1.));
#4915=DIRECTION('',(1.,0.,0.));
#4916=DIRECTION('',(0.,0.,1.));
#4917=DIRECTION('',(1.,0.,0.));
#4918=DIRECTION('',(0.,0.,1.));
#4919=DIRECTION('',(1.,0.,0.));
#4920=DIRECTION('',(0.,0.,1.));
#4921=DIRECTION('',(1.,0.,0.));
#4922=DIRECTION('',(0.,0.,1.));
#4923=DIRECTION('',(1.,0.,0.));
#4924=DIRECTION('',(0.,0.,1.));
#4925=DIRECTION('',(1.,0.,0.));
#4926=DIRECTION('',(0.,0.,1.));
#4927=DIRECTION('',(1.,0.,0.));
#4928=DIRECTION('',(0.,0.,1.));
#4929=DIRECTION('',(-1.,1.22464679914735E-16,0.));
#4930=DIRECTION('',(0.,0.,1.));
#4931=DIRECTION('',(-1.,1.22464679914735E-16,0.));
#4932=DIRECTION('',(0.,0.,1.));
#4933=DIRECTION('',(-1.,1.22464679914735E-16,0.));
#4934=DIRECTION('',(0.,0.,1.));
#4935=DIRECTION('',(-1.,1.22464679914735E-16,0.));
#4936=DIRECTION('',(0.,0.,1.));
#4937=DIRECTION('',(1.,0.,0.));
#4938=DIRECTION('',(0.,0.,1.));
#4939=DIRECTION('',(1.,0.,0.));
#4940=DIRECTION('',(0.,0.,1.));
#4941=DIRECTION('',(1.,0.,0.));
#4942=DIRECTION('',(0.,0.,1.));
#4943=DIRECTION('',(1.,0.,0.));
#4944=DIRECTION('',(0.,0.,1.));
#4945=DIRECTION('',(1.,0.,0.));
#4946=DIRECTION('',(0.,0.,1.));
#4947=DIRECTION('',(1.,0.,0.));
#4948=DIRECTION('',(0.,0.,1.));
#4949=DIRECTION('',(1.,0.,0.));
#4950=CARTESIAN_POINT('',(0.,0.,0.));
#4951=CARTESIAN_POINT('',(0.,0.,0.));
#4952=CARTESIAN_POINT('',(0.,0.,0.));
#4953=CARTESIAN_POINT('Origin',(-2.9,-2.,0.9));
#4954=CARTESIAN_POINT('',(-3.23,-2.,1.));
#4955=CARTESIAN_POINT('Origin',(-2.9,-2.,1.));
#4956=CARTESIAN_POINT('',(-3.23,-2.,1.8));
#4957=CARTESIAN_POINT('',(-3.23,-2.,0.9));
#4958=CARTESIAN_POINT('Origin',(-2.9,-2.,1.8));
#4959=CARTESIAN_POINT('Origin',(2.9,-2.,0.9));
#4960=CARTESIAN_POINT('',(2.57,-2.,1.));
#4961=CARTESIAN_POINT('Origin',(2.9,-2.,1.));
#4962=CARTESIAN_POINT('',(2.57,-2.,1.8));
#4963=CARTESIAN_POINT('',(2.57,-2.,0.9));
#4964=CARTESIAN_POINT('Origin',(2.9,-2.,1.8));
#4965=CARTESIAN_POINT('Origin',(0.,-2.5,4.5));
#4966=CARTESIAN_POINT('',(-0.505,-2.4,4.5));
#4967=CARTESIAN_POINT('Origin',(0.,-2.4,4.5));
#4968=CARTESIAN_POINT('',(-0.505,-1.6,4.5));
#4969=CARTESIAN_POINT('',(-0.505,-2.5,4.5));
#4970=CARTESIAN_POINT('Origin',(0.,-1.6,4.5));
#4971=CARTESIAN_POINT('Origin',(-3.5,-3.2,1.8));
#4972=CARTESIAN_POINT('',(3.5,-3.2,1.8));
#4973=CARTESIAN_POINT('',(-3.5,-3.2,1.8));
#4974=CARTESIAN_POINT('',(3.5,-3.2,1.8));
#4975=CARTESIAN_POINT('',(3.5,-0.8,1.8));
#4976=CARTESIAN_POINT('',(3.5,-3.2,1.8));
#4977=CARTESIAN_POINT('',(-3.5,-0.8,1.8));
#4978=CARTESIAN_POINT('',(3.5,-0.8,1.8));
#4979=CARTESIAN_POINT('',(-3.5,-3.2,1.8));
#4980=CARTESIAN_POINT('',(2.2,-1.6,1.8));
#4981=CARTESIAN_POINT('',(-2.2,-1.6,1.8));
#4982=CARTESIAN_POINT('',(-0.65,-1.6,1.8));
#4983=CARTESIAN_POINT('',(2.2,-2.4,1.8));
#4984=CARTESIAN_POINT('',(2.2,-2.8,1.8));
#4985=CARTESIAN_POINT('',(-2.2,-2.4,1.8));
#4986=CARTESIAN_POINT('',(-2.85,-2.4,1.8));
#4987=CARTESIAN_POINT('',(-2.2,-2.4,1.8));
#4988=CARTESIAN_POINT('Origin',(-3.5,-3.2,1.));
#4989=CARTESIAN_POINT('',(-3.5,-3.2,1.));
#4990=CARTESIAN_POINT('',(-3.5,-3.2,1.8));
#4991=CARTESIAN_POINT('',(-3.5,-0.8,1.));
#4992=CARTESIAN_POINT('',(-3.5,-0.8,1.8));
#4993=CARTESIAN_POINT('',(-3.5,-3.2,1.));
#4994=CARTESIAN_POINT('Origin',(3.5,-3.2,1.8));
#4995=CARTESIAN_POINT('',(3.5,-3.2,1.));
#4996=CARTESIAN_POINT('',(3.5,-3.2,1.));
#4997=CARTESIAN_POINT('',(3.5,-0.8,1.));
#4998=CARTESIAN_POINT('',(3.5,-3.2,1.));
#4999=CARTESIAN_POINT('',(3.5,-0.8,1.));
#5000=CARTESIAN_POINT('Origin',(0.,-0.8,1.4));
#5001=CARTESIAN_POINT('',(-3.5,-0.8,1.));
#5002=CARTESIAN_POINT('Origin',(0.,-3.2,1.4));
#5003=CARTESIAN_POINT('',(-3.5,-3.2,1.));
#5004=CARTESIAN_POINT('Origin',(-2.2,-2.4,1.));
#5005=CARTESIAN_POINT('',(2.2,-2.4,6.5));
#5006=CARTESIAN_POINT('',(2.2,-2.4,1.));
#5007=CARTESIAN_POINT('',(-2.2,-2.4,6.5));
#5008=CARTESIAN_POINT('',(-2.2,-2.4,6.5));
#5009=CARTESIAN_POINT('',(-2.2,-2.4,1.));
#5010=CARTESIAN_POINT('Origin',(2.2,-2.4,1.));
#5011=CARTESIAN_POINT('',(2.2,-1.6,6.5));
#5012=CARTESIAN_POINT('',(2.2,-1.6,1.));
#5013=CARTESIAN_POINT('',(2.2,-2.4,6.5));
#5014=CARTESIAN_POINT('Origin',(2.2,-1.6,1.));
#5015=CARTESIAN_POINT('',(-2.2,-1.6,6.5));
#5016=CARTESIAN_POINT('',(-2.2,-1.6,1.));
#5017=CARTESIAN_POINT('',(2.2,-1.6,6.5));
#5018=CARTESIAN_POINT('Origin',(-2.2,-1.6,1.));
#5019=CARTESIAN_POINT('',(-2.2,-1.6,6.5));
#5020=CARTESIAN_POINT('Origin',(0.,-2.,6.5));
#5021=CARTESIAN_POINT('Origin',(0.,-2.,1.));
#5022=CARTESIAN_POINT('',(0.,0.,0.));
#5023=CARTESIAN_POINT('Origin',(-2.9,32.,0.9));
#5024=CARTESIAN_POINT('',(-3.23,32.,1.));
#5025=CARTESIAN_POINT('Origin',(-2.9,32.,1.));
#5026=CARTESIAN_POINT('',(-3.23,32.,1.8));
#5027=CARTESIAN_POINT('',(-3.23,32.,0.9));
#5028=CARTESIAN_POINT('Origin',(-2.9,32.,1.8));
#5029=CARTESIAN_POINT('Origin',(2.9,32.,0.9));
#5030=CARTESIAN_POINT('',(2.57,32.,1.));
#5031=CARTESIAN_POINT('Origin',(2.9,32.,1.));
#5032=CARTESIAN_POINT('',(2.57,32.,1.8));
#5033=CARTESIAN_POINT('',(2.57,32.,0.9));
#5034=CARTESIAN_POINT('Origin',(2.9,32.,1.8));
#5035=CARTESIAN_POINT('Origin',(0.,31.5,4.5));
#5036=CARTESIAN_POINT('',(-0.505,31.6,4.5));
#5037=CARTESIAN_POINT('Origin',(0.,31.6,4.5));
#5038=CARTESIAN_POINT('',(-0.505,32.4,4.5));
#5039=CARTESIAN_POINT('',(-0.505,31.5,4.5));
#5040=CARTESIAN_POINT('Origin',(0.,32.4,4.5));
#5041=CARTESIAN_POINT('Origin',(-3.5,30.8,1.8));
#5042=CARTESIAN_POINT('',(3.5,30.8,1.8));
#5043=CARTESIAN_POINT('',(-3.5,30.8,1.8));
#5044=CARTESIAN_POINT('',(3.5,30.8,1.8));
#5045=CARTESIAN_POINT('',(3.5,33.2,1.8));
#5046=CARTESIAN_POINT('',(3.5,30.8,1.8));
#5047=CARTESIAN_POINT('',(-3.5,33.2,1.8));
#5048=CARTESIAN_POINT('',(3.5,33.2,1.8));
#5049=CARTESIAN_POINT('',(-3.5,30.8,1.8));
#5050=CARTESIAN_POINT('',(2.2,32.4,1.8));
#5051=CARTESIAN_POINT('',(-2.2,32.4,1.8));
#5052=CARTESIAN_POINT('',(-0.65,32.4,1.8));
#5053=CARTESIAN_POINT('',(2.2,31.6,1.8));
#5054=CARTESIAN_POINT('',(2.2,31.2,1.8));
#5055=CARTESIAN_POINT('',(-2.2,31.6,1.8));
#5056=CARTESIAN_POINT('',(-2.85,31.6,1.8));
#5057=CARTESIAN_POINT('',(-2.2,31.6,1.8));
#5058=CARTESIAN_POINT('Origin',(-3.5,30.8,1.));
#5059=CARTESIAN_POINT('',(-3.5,30.8,1.));
#5060=CARTESIAN_POINT('',(-3.5,30.8,1.8));
#5061=CARTESIAN_POINT('',(-3.5,33.2,1.));
#5062=CARTESIAN_POINT('',(-3.5,33.2,1.8));
#5063=CARTESIAN_POINT('',(-3.5,30.8,1.));
#5064=CARTESIAN_POINT('Origin',(3.5,30.8,1.8));
#5065=CARTESIAN_POINT('',(3.5,30.8,1.));
#5066=CARTESIAN_POINT('',(3.5,30.8,1.));
#5067=CARTESIAN_POINT('',(3.5,33.2,1.));
#5068=CARTESIAN_POINT('',(3.5,30.8,1.));
#5069=CARTESIAN_POINT('',(3.5,33.2,1.));
#5070=CARTESIAN_POINT('Origin',(0.,33.2,1.4));
#5071=CARTESIAN_POINT('',(-3.5,33.2,1.));
#5072=CARTESIAN_POINT('Origin',(0.,30.8,1.4));
#5073=CARTESIAN_POINT('',(-3.5,30.8,1.));
#5074=CARTESIAN_POINT('Origin',(-2.2,31.6,1.));
#5075=CARTESIAN_POINT('',(2.2,31.6,6.5));
#5076=CARTESIAN_POINT('',(2.2,31.6,1.));
#5077=CARTESIAN_POINT('',(-2.2,31.6,6.5));
#5078=CARTESIAN_POINT('',(-2.2,31.6,6.5));
#5079=CARTESIAN_POINT('',(-2.2,31.6,1.));
#5080=CARTESIAN_POINT('Origin',(2.2,31.6,1.));
#5081=CARTESIAN_POINT('',(2.2,32.4,6.5));
#5082=CARTESIAN_POINT('',(2.2,32.4,1.));
#5083=CARTESIAN_POINT('',(2.2,31.6,6.5));
#5084=CARTESIAN_POINT('Origin',(2.2,32.4,1.));
#5085=CARTESIAN_POINT('',(-2.2,32.4,6.5));
#5086=CARTESIAN_POINT('',(-2.2,32.4,1.));
#5087=CARTESIAN_POINT('',(2.2,32.4,6.5));
#5088=CARTESIAN_POINT('Origin',(-2.2,32.4,1.));
#5089=CARTESIAN_POINT('',(-2.2,32.4,6.5));
#5090=CARTESIAN_POINT('Origin',(0.,32.,6.5));
#5091=CARTESIAN_POINT('Origin',(0.,32.,1.));
#5092=CARTESIAN_POINT('',(0.,0.,0.));
#5093=CARTESIAN_POINT('Origin',(0.,30.8,4.5));
#5094=CARTESIAN_POINT('',(-0.165,30.8,4.5));
#5095=CARTESIAN_POINT('Origin',(0.,30.8,4.5));
#5096=CARTESIAN_POINT('',(-0.165,32.5,4.5));
#5097=CARTESIAN_POINT('',(-0.165,30.8,4.5));
#5098=CARTESIAN_POINT('Origin',(0.,32.5,4.5));
#5099=CARTESIAN_POINT('Origin',(0.,30.8,4.5));
#5100=CARTESIAN_POINT('Origin',(0.,-2.6,4.5));
#5101=CARTESIAN_POINT('',(-0.165,-2.5,4.5));
#5102=CARTESIAN_POINT('Origin',(0.,-2.5,4.5));
#5103=CARTESIAN_POINT('',(-0.165,-0.8,4.5));
#5104=CARTESIAN_POINT('',(-0.165,-2.6,4.5));
#5105=CARTESIAN_POINT('Origin',(0.,-0.8,4.5));
#5106=CARTESIAN_POINT('Origin',(0.,-0.8,4.5));
#5107=CARTESIAN_POINT('Origin',(0.,29.1,4.5));
#5108=CARTESIAN_POINT('',(-0.6,29.1,4.5));
#5109=CARTESIAN_POINT('Origin',(0.,29.1,4.5));
#5110=CARTESIAN_POINT('',(-0.5,29.1,4.5));
#5111=CARTESIAN_POINT('Origin',(0.,29.1,4.5));
#5112=CARTESIAN_POINT('Origin',(0.,0.9,4.5));
#5113=CARTESIAN_POINT('',(-0.6,0.9,4.5));
#5114=CARTESIAN_POINT('Origin',(0.,0.9,4.5));
#5115=CARTESIAN_POINT('',(-0.5,0.9,4.5));
#5116=CARTESIAN_POINT('Origin',(0.,0.9,4.5));
#5117=CARTESIAN_POINT('Origin',(0.,0.9,4.5));
#5118=CARTESIAN_POINT('',(-0.6,0.9,4.5));
#5119=CARTESIAN_POINT('Origin',(0.,-2.5,4.5));
#5120=CARTESIAN_POINT('',(-0.5,-2.5,4.5));
#5121=CARTESIAN_POINT('',(-0.5,-2.5,4.5));
#5122=CARTESIAN_POINT('Origin',(0.,-2.5,4.5));
#5123=CARTESIAN_POINT('Origin',(0.,-2.5,4.5));
#5124=CARTESIAN_POINT('',(-0.5,32.5,4.5));
#5125=CARTESIAN_POINT('Origin',(0.,32.5,4.5));
#5126=CARTESIAN_POINT('',(-0.5,-2.5,4.5));
#5127=CARTESIAN_POINT('Origin',(0.,32.5,4.5));
#5128=CARTESIAN_POINT('Origin',(0.,-2.5,4.5));
#5129=CARTESIAN_POINT('',(0.,0.,0.));
#5130=CARTESIAN_POINT('Origin',(0.,-1.6,4.5));
#5131=CARTESIAN_POINT('',(-0.505,0.,4.5));
#5132=CARTESIAN_POINT('Origin',(0.,0.,4.5));
#5133=CARTESIAN_POINT('',(-0.505,-1.6,4.5));
#5134=CARTESIAN_POINT('',(-0.505,-1.6,4.5));
#5135=CARTESIAN_POINT('Origin',(0.,-1.6,4.5));
#5136=CARTESIAN_POINT('Origin',(0.,-1.6,4.5));
#5137=CARTESIAN_POINT('',(-0.8,0.,4.5));
#5138=CARTESIAN_POINT('Origin',(0.,0.,4.5));
#5139=CARTESIAN_POINT('',(-0.8,-1.6,4.5));
#5140=CARTESIAN_POINT('',(-0.8,-1.6,4.5));
#5141=CARTESIAN_POINT('Origin',(0.,-1.6,4.5));
#5142=CARTESIAN_POINT('Origin',(0.,0.,4.5));
#5143=CARTESIAN_POINT('Origin',(0.,-1.6,4.5));
#5144=CARTESIAN_POINT('',(0.,0.,0.));
#5145=CARTESIAN_POINT('Origin',(0.,30.,4.5));
#5146=CARTESIAN_POINT('',(-0.505,31.6,4.5));
#5147=CARTESIAN_POINT('Origin',(0.,31.6,4.5));
#5148=CARTESIAN_POINT('',(-0.505,30.,4.5));
#5149=CARTESIAN_POINT('',(-0.505,30.,4.5));
#5150=CARTESIAN_POINT('Origin',(0.,30.,4.5));
#5151=CARTESIAN_POINT('Origin',(0.,30.,4.5));
#5152=CARTESIAN_POINT('',(-0.8,31.6,4.5));
#5153=CARTESIAN_POINT('Origin',(0.,31.6,4.5));
#5154=CARTESIAN_POINT('',(-0.8,30.,4.5));
#5155=CARTESIAN_POINT('',(-0.8,30.,4.5));
#5156=CARTESIAN_POINT('Origin',(0.,30.,4.5));
#5157=CARTESIAN_POINT('Origin',(0.,31.6,4.5));
#5158=CARTESIAN_POINT('Origin',(0.,30.,4.5));
#5159=CARTESIAN_POINT('',(0.,0.,0.));
#5160=CARTESIAN_POINT('Origin',(2.9,-2.,-0.1));
#5161=CARTESIAN_POINT('',(2.65,-2.,0.));
#5162=CARTESIAN_POINT('Origin',(2.9,-2.,0.));
#5163=CARTESIAN_POINT('',(2.65,-2.,1.));
#5164=CARTESIAN_POINT('',(2.65,-2.,-0.1));
#5165=CARTESIAN_POINT('Origin',(2.9,-2.,1.));
#5166=CARTESIAN_POINT('Origin',(-2.9,32.,-0.1));
#5167=CARTESIAN_POINT('',(-3.15,32.,0.));
#5168=CARTESIAN_POINT('Origin',(-2.9,32.,0.));
#5169=CARTESIAN_POINT('',(-3.15,32.,1.));
#5170=CARTESIAN_POINT('',(-3.15,32.,-0.1));
#5171=CARTESIAN_POINT('Origin',(-2.9,32.,1.));
#5172=CARTESIAN_POINT('Origin',(-2.9,-2.,-0.1));
#5173=CARTESIAN_POINT('',(-3.15,-2.,0.));
#5174=CARTESIAN_POINT('Origin',(-2.9,-2.,0.));
#5175=CARTESIAN_POINT('',(-3.15,-2.,1.));
#5176=CARTESIAN_POINT('',(-3.15,-2.,-0.1));
#5177=CARTESIAN_POINT('Origin',(-2.9,-2.,1.));
#5178=CARTESIAN_POINT('Origin',(2.9,32.,-0.1));
#5179=CARTESIAN_POINT('',(2.65,32.,0.));
#5180=CARTESIAN_POINT('Origin',(2.9,32.,0.));
#5181=CARTESIAN_POINT('',(2.65,32.,1.));
#5182=CARTESIAN_POINT('',(2.65,32.,-0.1));
#5183=CARTESIAN_POINT('Origin',(2.9,32.,1.));
#5184=CARTESIAN_POINT('Origin',(4.5,34.,0.));
#5185=CARTESIAN_POINT('',(4.5,34.,0.));
#5186=CARTESIAN_POINT('',(-4.5,34.,0.));
#5187=CARTESIAN_POINT('',(4.5,34.,0.));
#5188=CARTESIAN_POINT('',(-4.5,34.,1.));
#5189=CARTESIAN_POINT('',(-4.5,34.,0.));
#5190=CARTESIAN_POINT('',(4.5,34.,1.));
#5191=CARTESIAN_POINT('',(4.5,34.,1.));
#5192=CARTESIAN_POINT('',(4.5,34.,0.));
#5193=CARTESIAN_POINT('Origin',(4.5,-4.,0.));
#5194=CARTESIAN_POINT('',(4.5,-4.,0.));
#5195=CARTESIAN_POINT('',(4.5,-4.,0.));
#5196=CARTESIAN_POINT('',(4.5,-4.,1.));
#5197=CARTESIAN_POINT('',(4.5,-4.,1.));
#5198=CARTESIAN_POINT('',(4.5,-4.,0.));
#5199=CARTESIAN_POINT('Origin',(-4.5,-4.,0.));
#5200=CARTESIAN_POINT('',(-4.5,-4.,0.));
#5201=CARTESIAN_POINT('',(-4.5,-4.,0.));
#5202=CARTESIAN_POINT('',(-4.5,-4.,1.));
#5203=CARTESIAN_POINT('',(-4.5,-4.,1.));
#5204=CARTESIAN_POINT('',(-4.5,-4.,0.));
#5205=CARTESIAN_POINT('Origin',(-4.5,34.,0.));
#5206=CARTESIAN_POINT('',(-4.5,34.,0.));
#5207=CARTESIAN_POINT('',(-4.5,34.,1.));
#5208=CARTESIAN_POINT('Origin',(0.,15.,1.));
#5209=CARTESIAN_POINT('Origin',(0.,15.,0.));
#5210=CARTESIAN_POINT('',(0.,0.,0.));
#5211=CARTESIAN_POINT('Origin',(4.5,-3.,-0.3));
#5212=CARTESIAN_POINT('',(4.5,-3.,-0.3));
#5213=CARTESIAN_POINT('',(-4.5,-3.,-0.3));
#5214=CARTESIAN_POINT('',(4.5,-3.,-0.3));
#5215=CARTESIAN_POINT('',(-4.5,-3.,0.));
#5216=CARTESIAN_POINT('',(-4.5,-3.,-0.3));
#5217=CARTESIAN_POINT('',(4.5,-3.,0.));
#5218=CARTESIAN_POINT('',(4.5,-3.,0.));
#5219=CARTESIAN_POINT('',(4.5,-3.,-0.3));
#5220=CARTESIAN_POINT('Origin',(4.5,-4.,-0.3));
#5221=CARTESIAN_POINT('',(4.5,-4.,-0.3));
#5222=CARTESIAN_POINT('',(4.5,-4.,-0.3));
#5223=CARTESIAN_POINT('',(4.5,-4.,0.));
#5224=CARTESIAN_POINT('',(4.5,-4.,0.));
#5225=CARTESIAN_POINT('',(4.5,-4.,-0.3));
#5226=CARTESIAN_POINT('Origin',(-4.5,-4.,-0.3));
#5227=CARTESIAN_POINT('',(-4.5,-4.,-0.3));
#5228=CARTESIAN_POINT('',(-4.5,-4.,-0.3));
#5229=CARTESIAN_POINT('',(-4.5,-4.,0.));
#5230=CARTESIAN_POINT('',(-4.5,-4.,0.));
#5231=CARTESIAN_POINT('',(-4.5,-4.,-0.3));
#5232=CARTESIAN_POINT('Origin',(-4.5,-3.,-0.3));
#5233=CARTESIAN_POINT('',(-4.5,-3.,-0.3));
#5234=CARTESIAN_POINT('',(-4.5,-3.,0.));
#5235=CARTESIAN_POINT('Origin',(0.,-3.5,0.));
#5236=CARTESIAN_POINT('Origin',(0.,-3.5,-0.3));
#5237=CARTESIAN_POINT('',(0.,0.,0.));
#5238=CARTESIAN_POINT('Origin',(0.,0.,0.));
#5239=CARTESIAN_POINT('',(-0.32,0.16,3.91886975727153E-17));
#5240=CARTESIAN_POINT('Origin',(0.,0.16,0.));
#5241=CARTESIAN_POINT('',(-0.32,0.,3.91886975727153E-17));
#5242=CARTESIAN_POINT('',(-0.32,0.,3.91886975727153E-17));
#5243=CARTESIAN_POINT('Origin',(0.,0.,0.));
#5244=CARTESIAN_POINT('Origin',(0.,0.,0.));
#5245=CARTESIAN_POINT('',(-0.6,0.16,7.34788079488412E-17));
#5246=CARTESIAN_POINT('Origin',(0.,0.16,0.));
#5247=CARTESIAN_POINT('',(-0.6,0.,7.34788079488412E-17));
#5248=CARTESIAN_POINT('',(-0.6,0.,7.34788079488412E-17));
#5249=CARTESIAN_POINT('Origin',(0.,0.,0.));
#5250=CARTESIAN_POINT('Origin',(0.,0.16,0.));
#5251=CARTESIAN_POINT('Origin',(0.,0.,0.));
#5252=CARTESIAN_POINT('',(0.,0.,0.));
#5253=CARTESIAN_POINT('Origin',(0.144337567297406,-0.6,-0.25));
#5254=CARTESIAN_POINT('',(0.288675134594813,-0.6,0.));
#5255=CARTESIAN_POINT('',(0.144337567297406,-0.6,-0.25));
#5256=CARTESIAN_POINT('',(0.288675134594813,-0.6,0.));
#5257=CARTESIAN_POINT('',(0.144337567297406,-0.96,-0.25));
#5258=CARTESIAN_POINT('',(0.144337567297406,-0.6,-0.25));
#5259=CARTESIAN_POINT('',(0.288675134594813,-0.96,0.));
#5260=CARTESIAN_POINT('',(0.288675134594813,-0.96,0.));
#5261=CARTESIAN_POINT('',(0.288675134594813,-0.6,0.));
#5262=CARTESIAN_POINT('Origin',(-0.144337567297406,-0.6,-0.25));
#5263=CARTESIAN_POINT('',(-0.144337567297406,-0.6,-0.25));
#5264=CARTESIAN_POINT('',(0.144337567297406,-0.6,-0.25));
#5265=CARTESIAN_POINT('',(-0.144337567297406,-0.96,-0.25));
#5266=CARTESIAN_POINT('',(-0.144337567297406,-0.6,-0.25));
#5267=CARTESIAN_POINT('',(0.144337567297406,-0.96,-0.25));
#5268=CARTESIAN_POINT('Origin',(-0.288675134594813,-0.6,-8.32667268468867E-17));
#5269=CARTESIAN_POINT('',(-0.288675134594813,-0.6,-3.53525079574969E-17));
#5270=CARTESIAN_POINT('',(-0.144337567297406,-0.6,-0.25));
#5271=CARTESIAN_POINT('',(-0.288675134594813,-0.96,-5.55111512312578E-17));
#5272=CARTESIAN_POINT('',(-0.288675134594813,-0.6,-3.53525079574969E-17));
#5273=CARTESIAN_POINT('',(-0.144337567297406,-0.96,-0.25));
#5274=CARTESIAN_POINT('Origin',(-0.144337567297407,-0.6,0.25));
#5275=CARTESIAN_POINT('',(-0.144337567297407,-0.6,0.25));
#5276=CARTESIAN_POINT('',(-0.288675134594813,-0.6,-3.53525079574969E-17));
#5277=CARTESIAN_POINT('',(-0.144337567297407,-0.96,0.25));
#5278=CARTESIAN_POINT('',(-0.144337567297407,-0.6,0.25));
#5279=CARTESIAN_POINT('',(-0.288675134594813,-0.96,-3.53525079574969E-17));
#5280=CARTESIAN_POINT('Origin',(0.144337567297406,-0.6,0.25));
#5281=CARTESIAN_POINT('',(0.144337567297406,-0.6,0.25));
#5282=CARTESIAN_POINT('',(-0.144337567297407,-0.6,0.25));
#5283=CARTESIAN_POINT('',(0.144337567297406,-0.96,0.25));
#5284=CARTESIAN_POINT('',(0.144337567297406,-0.6,0.25));
#5285=CARTESIAN_POINT('',(-0.144337567297407,-0.96,0.25));
#5286=CARTESIAN_POINT('Origin',(0.288675134594813,-0.6,0.));
#5287=CARTESIAN_POINT('',(0.144337567297406,-0.6,0.25));
#5288=CARTESIAN_POINT('',(0.144337567297406,-0.96,0.25));
#5289=CARTESIAN_POINT('Origin',(0.,-0.6,0.));
#5290=CARTESIAN_POINT('Origin',(0.,-0.96,0.));
#5291=CARTESIAN_POINT('Origin',(0.,-1.8,0.));
#5292=CARTESIAN_POINT('',(-0.2942,-1.8,3.60291088309151E-17));
#5293=CARTESIAN_POINT('Origin',(0.,-1.8,0.));
#5294=CARTESIAN_POINT('Origin',(0.45,0.6,0.));
#5295=CARTESIAN_POINT('',(-0.45,0.6,-5.51091059616309E-17));
#5296=CARTESIAN_POINT('Origin',(0.,0.6,0.));
#5297=CARTESIAN_POINT('Origin',(0.,0.575,0.));
#5298=CARTESIAN_POINT('',(-0.5,0.55,-6.12323399573677E-17));
#5299=CARTESIAN_POINT('Origin',(0.,0.55,0.));
#5300=CARTESIAN_POINT('',(-0.475,0.575,-5.81707229594993E-17));
#5301=CARTESIAN_POINT('Origin',(0.,0.29,0.));
#5302=CARTESIAN_POINT('',(-0.5,0.0299999999999998,-6.12323399573677E-17));
#5303=CARTESIAN_POINT('Origin',(0.,0.0299999999999998,0.));
#5304=CARTESIAN_POINT('',(-0.5,0.29,-6.12323399573677E-17));
#5305=CARTESIAN_POINT('Origin',(0.,0.0150000000000001,0.));
#5306=CARTESIAN_POINT('',(-0.47,7.11236625150491E-17,-5.75583995599256E-17));
#5307=CARTESIAN_POINT('Origin',(0.,0.,0.));
#5308=CARTESIAN_POINT('',(-0.485,0.0150000000000001,-5.93953697586466E-17));
#5309=CARTESIAN_POINT('Origin',(0.32,0.,0.));
#5310=CARTESIAN_POINT('',(-0.32,-6.93889390390723E-18,-3.91886975727153E-17));
#5311=CARTESIAN_POINT('Origin',(0.,0.,0.));
#5312=CARTESIAN_POINT('Origin',(0.,-0.02,0.));
#5313=CARTESIAN_POINT('',(-0.2942,-0.0515999999999999,3.60291088309151E-17));
#5314=CARTESIAN_POINT('Origin',(0.,-0.0515999999999999,0.));
#5315=CARTESIAN_POINT('',(-0.31,-0.02,-3.7964050773568E-17));
#5316=CARTESIAN_POINT('Origin',(0.,-1.24,0.));
#5317=CARTESIAN_POINT('',(-0.2942,-1.24,-3.60291088309151E-17));
#5318=CARTESIAN_POINT('',(0.,0.,0.));
#5319=CARTESIAN_POINT('Origin',(0.,-2.8,4.5));
#5320=CARTESIAN_POINT('',(-0.225,-2.5,4.5));
#5321=CARTESIAN_POINT('Origin',(0.,-2.5,4.5));
#5322=CARTESIAN_POINT('',(-0.225,-2.8,4.5));
#5323=CARTESIAN_POINT('',(-0.225,-2.8,4.5));
#5324=CARTESIAN_POINT('Origin',(0.,-2.8,4.5));
#5325=CARTESIAN_POINT('Origin',(0.,-2.8,4.5));
#5326=CARTESIAN_POINT('',(-1.1,-2.5,4.5));
#5327=CARTESIAN_POINT('Origin',(0.,-2.5,4.5));
#5328=CARTESIAN_POINT('',(-1.1,-2.8,4.5));
#5329=CARTESIAN_POINT('',(-1.1,-2.8,4.5));
#5330=CARTESIAN_POINT('Origin',(0.,-2.8,4.5));
#5331=CARTESIAN_POINT('Origin',(0.,-2.5,4.5));
#5332=CARTESIAN_POINT('Origin',(0.,-2.8,4.5));
#5333=CARTESIAN_POINT('',(0.,0.,0.));
#5334=CARTESIAN_POINT('Origin',(0.,-2.5,4.5));
#5335=CARTESIAN_POINT('',(-0.605,-2.4,4.5));
#5336=CARTESIAN_POINT('Origin',(0.,-2.4,4.5));
#5337=CARTESIAN_POINT('',(-0.605,-2.5,4.5));
#5338=CARTESIAN_POINT('',(-0.605,-2.5,4.5));
#5339=CARTESIAN_POINT('Origin',(0.,-2.5,4.5));
#5340=CARTESIAN_POINT('Origin',(0.,-2.5,4.5));
#5341=CARTESIAN_POINT('',(-1.,-2.4,4.5));
#5342=CARTESIAN_POINT('Origin',(0.,-2.4,4.5));
#5343=CARTESIAN_POINT('',(-1.,-2.5,4.5));
#5344=CARTESIAN_POINT('',(-1.,-2.5,4.5));
#5345=CARTESIAN_POINT('Origin',(0.,-2.5,4.5));
#5346=CARTESIAN_POINT('Origin',(0.,-2.4,4.5));
#5347=CARTESIAN_POINT('Origin',(0.,-2.5,4.5));
#5348=CARTESIAN_POINT('',(0.,0.,0.));
#5349=CARTESIAN_POINT('',(0.,0.,0.));
#5350=CARTESIAN_POINT('Origin',(0.,0.,0.));
#5351=CARTESIAN_POINT('',(-0.976185,-0.246528389340863,-1.19548183562566E-16));
#5352=CARTESIAN_POINT('',(-1.19548183562566E-16,-0.246528389340863,0.976185));
#5353=CARTESIAN_POINT('Origin',(0.,-0.246528389340863,0.));
#5354=CARTESIAN_POINT('Origin',(0.,-0.246528389340863,0.));
#5355=CARTESIAN_POINT('',(-1.19548183562566E-16,0.246528389340863,0.976185));
#5356=CARTESIAN_POINT('Origin',(-1.22464679914735E-16,0.,1.));
#5357=CARTESIAN_POINT('',(-0.976185,0.246528389340863,1.19548183562566E-16));
#5358=CARTESIAN_POINT('Origin',(0.,0.246528389340863,0.));
#5359=CARTESIAN_POINT('Origin',(0.,0.246528389340863,0.));
#5360=CARTESIAN_POINT('Origin',(0.,0.,0.));
#5361=CARTESIAN_POINT('',(-0.976185,0.45,-1.19548183562566E-16));
#5362=CARTESIAN_POINT('',(-0.976185,0.,-1.19548183562566E-16));
#5363=CARTESIAN_POINT('Origin',(0.,0.45,0.));
#5364=CARTESIAN_POINT('Origin',(0.,0.,0.));
#5365=CARTESIAN_POINT('',(-0.5,-0.39,-6.12323399573677E-17));
#5366=CARTESIAN_POINT('Origin',(0.,-0.39,0.));
#5367=CARTESIAN_POINT('',(-0.5,0.39,-6.12323399573677E-17));
#5368=CARTESIAN_POINT('',(-0.5,0.,-6.12323399573677E-17));
#5369=CARTESIAN_POINT('Origin',(0.,0.39,0.));
#5370=CARTESIAN_POINT('Origin',(0.,0.42,0.));
#5371=CARTESIAN_POINT('',(-0.56,0.45,-6.85802207522518E-17));
#5372=CARTESIAN_POINT('',(-0.53,0.42,-6.49062803548097E-17));
#5373=CARTESIAN_POINT('Origin',(0.,0.45,0.));
#5374=CARTESIAN_POINT('Origin',(0.976185,0.45,0.));
#5375=CARTESIAN_POINT('Origin',(0.,0.,0.));
#5376=CARTESIAN_POINT('',(-0.976185,-0.45,-1.19548183562566E-16));
#5377=CARTESIAN_POINT('Origin',(0.,-0.45,0.));
#5378=CARTESIAN_POINT('',(-0.976185,0.,-1.19548183562566E-16));
#5379=CARTESIAN_POINT('Origin',(0.56,-0.45,0.));
#5380=CARTESIAN_POINT('',(-0.56,-0.45,-6.85802207522518E-17));
#5381=CARTESIAN_POINT('Origin',(0.,-0.45,0.));
#5382=CARTESIAN_POINT('Origin',(0.,-0.42,0.));
#5383=CARTESIAN_POINT('',(-0.53,-0.42,-6.49062803548097E-17));
#5384=CARTESIAN_POINT('',(0.,0.,0.));
#5385=CARTESIAN_POINT('Origin',(0.,0.,0.));
#5386=CARTESIAN_POINT('',(-1.023815,0.246528389340863,-1.25381176266905E-16));
#5387=CARTESIAN_POINT('',(-1.25381176266905E-16,0.246528389340863,1.023815));
#5388=CARTESIAN_POINT('Origin',(0.,0.246528389340863,0.));
#5389=CARTESIAN_POINT('Origin',(0.,0.246528389340863,0.));
#5390=CARTESIAN_POINT('',(-1.25381176266905E-16,-0.246528389340863,1.023815));
#5391=CARTESIAN_POINT('Origin',(-1.22464679914735E-16,0.,1.));
#5392=CARTESIAN_POINT('',(-1.023815,-0.246528389340863,1.25381176266905E-16));
#5393=CARTESIAN_POINT('Origin',(0.,-0.246528389340863,0.));
#5394=CARTESIAN_POINT('Origin',(0.,-0.246528389340863,0.));
#5395=CARTESIAN_POINT('Origin',(0.,0.,0.));
#5396=CARTESIAN_POINT('',(-1.023815,-0.45,-1.25381176266905E-16));
#5397=CARTESIAN_POINT('Origin',(0.,-0.45,0.));
#5398=CARTESIAN_POINT('',(-1.023815,0.,-1.25381176266905E-16));
#5399=CARTESIAN_POINT('Origin',(1.44,0.45,0.));
#5400=CARTESIAN_POINT('',(-1.44,0.45,-1.76349139077219E-16));
#5401=CARTESIAN_POINT('Origin',(0.,0.45,0.));
#5402=CARTESIAN_POINT('',(-1.023815,0.45,-1.25381176266905E-16));
#5403=CARTESIAN_POINT('Origin',(0.,0.45,0.));
#5404=CARTESIAN_POINT('Origin',(0.,0.42,0.));
#5405=CARTESIAN_POINT('',(-1.5,0.39,-1.83697019872103E-16));
#5406=CARTESIAN_POINT('Origin',(0.,0.39,0.));
#5407=CARTESIAN_POINT('',(-1.47,0.42,-1.80023079474661E-16));
#5408=CARTESIAN_POINT('Origin',(0.,0.,0.));
#5409=CARTESIAN_POINT('',(-1.5,-0.39,-1.83697019872103E-16));
#5410=CARTESIAN_POINT('Origin',(0.,-0.39,0.));
#5411=CARTESIAN_POINT('',(-1.5,0.,-1.83697019872103E-16));
#5412=CARTESIAN_POINT('Origin',(0.,-0.42,0.));
#5413=CARTESIAN_POINT('',(-1.44,-0.45,-1.76349139077219E-16));
#5414=CARTESIAN_POINT('Origin',(0.,-0.45,0.));
#5415=CARTESIAN_POINT('',(-1.47,-0.42,-1.80023079474661E-16));
#5416=CARTESIAN_POINT('Origin',(1.023815,-0.45,0.));
#5417=CARTESIAN_POINT('Origin',(0.,0.,0.));
#5418=CARTESIAN_POINT('',(-1.023815,0.,-1.25381176266905E-16));
#5419=CARTESIAN_POINT('',(0.,0.,0.));
#5420=CARTESIAN_POINT('Origin',(1.,0.,0.));
#5421=CARTESIAN_POINT('',(1.,-1.78583896120461E-33,0.23815));
#5422=CARTESIAN_POINT('',(1.,-1.78583896120461E-33,-0.23815));
#5423=CARTESIAN_POINT('Origin',(1.,0.,0.));
#5424=CARTESIAN_POINT('Origin',(0.707106781186548,0.,-0.707106781186547));
#5425=CARTESIAN_POINT('',(0.875504261126124,-1.78583896120461E-33,-0.538709301246971));
#5426=CARTESIAN_POINT('',(0.538709301246971,-1.78583896120461E-33,-0.875504261126124));
#5427=CARTESIAN_POINT('Origin',(0.707106781186548,0.,-0.707106781186547));
#5428=CARTESIAN_POINT('Origin',(6.12323399573677E-17,0.,-1.));
#5429=CARTESIAN_POINT('',(0.23815,-1.78583896120461E-33,-1.));
#5430=CARTESIAN_POINT('',(-0.23815,-1.78583896120461E-33,-1.));
#5431=CARTESIAN_POINT('Origin',(6.12323399573677E-17,0.,-1.));
#5432=CARTESIAN_POINT('Origin',(-0.707106781186547,0.,-0.707106781186548));
#5433=CARTESIAN_POINT('',(-0.538709301246971,-1.78583896120461E-33,-0.875504261126124));
#5434=CARTESIAN_POINT('',(-0.875504261126124,-1.78583896120461E-33,-0.538709301246971));
#5435=CARTESIAN_POINT('Origin',(-0.707106781186547,0.,-0.707106781186548));
#5436=CARTESIAN_POINT('Origin',(-1.,0.,-1.22464679914735E-16));
#5437=CARTESIAN_POINT('',(-1.,-1.78583896120461E-33,-0.23815));
#5438=CARTESIAN_POINT('',(-1.,-1.78583896120461E-33,0.23815));
#5439=CARTESIAN_POINT('Origin',(-1.,0.,-1.22464679914735E-16));
#5440=CARTESIAN_POINT('Origin',(-0.707106781186548,0.,0.707106781186547));
#5441=CARTESIAN_POINT('',(-0.875504261126124,-7.94881478324376E-33,0.538709301246971));
#5442=CARTESIAN_POINT('',(-0.538709301246971,4.37713686083455E-33,0.875504261126124));
#5443=CARTESIAN_POINT('Origin',(-0.707106781186548,0.,0.707106781186547));
#5444=CARTESIAN_POINT('Origin',(-1.83697019872103E-16,0.,1.));
#5445=CARTESIAN_POINT('',(-0.23815,-1.78583896120461E-33,1.));
#5446=CARTESIAN_POINT('',(0.23815,-1.78583896120461E-33,1.));
#5447=CARTESIAN_POINT('Origin',(-1.83697019872103E-16,0.,1.));
#5448=CARTESIAN_POINT('Origin',(0.707106781186547,0.,0.707106781186548));
#5449=CARTESIAN_POINT('',(0.538709301246971,-4.86732687222419E-33,0.875504261126124));
#5450=CARTESIAN_POINT('',(0.875504261126124,1.29564894981497E-33,0.538709301246971));
#5451=CARTESIAN_POINT('Origin',(0.707106781186547,0.,0.707106781186548));
#5452=CARTESIAN_POINT('',(0.,0.,0.));
#5453=CARTESIAN_POINT('Origin',(0.707106781186547,0.,0.707106781186548));
#5454=CARTESIAN_POINT('',(0.504455939115715,-0.04763,0.841298510752802));
#5455=CARTESIAN_POINT('',(0.841298510752802,-0.04763,0.504455939115715));
#5456=CARTESIAN_POINT('Ctrl Pts',(0.504455939115715,-0.04763,0.841298510752802));
#5457=CARTESIAN_POINT('Ctrl Pts',(0.508899795931835,-0.0740444353928835,
0.838633903678357));
#5458=CARTESIAN_POINT('Ctrl Pts',(0.517157748491652,-0.0999305678883309,
0.833661031856294));
#5459=CARTESIAN_POINT('Ctrl Pts',(0.537715343527944,-0.142345102874864,
0.820511285096538));
#5460=CARTESIAN_POINT('Ctrl Pts',(0.548874290046456,-0.159766064500479,
0.813159949759));
#5461=CARTESIAN_POINT('Ctrl Pts',(0.573915184558107,-0.190326085855194,
0.795684265985089));
#5462=CARTESIAN_POINT('Ctrl Pts',(0.587792702767295,-0.203463743702801,
0.78555112003688));
#5463=CARTESIAN_POINT('Ctrl Pts',(0.615966552324775,-0.224161999508995,
0.763642258217233));
#5464=CARTESIAN_POINT('Ctrl Pts',(0.631684198665438,-0.232861760990032,
0.750785745543687));
#5465=CARTESIAN_POINT('Ctrl Pts',(0.663382628119203,-0.244251601209411,
0.722929908501543));
#5466=CARTESIAN_POINT('Ctrl Pts',(0.679352081686668,-0.246942143572133,
0.707917883896095));
#5467=CARTESIAN_POINT('Ctrl Pts',(0.707917883896095,-0.246942143572133,
0.679352081686668));
#5468=CARTESIAN_POINT('Ctrl Pts',(0.722929908501543,-0.244251601209411,
0.663382628119203));
#5469=CARTESIAN_POINT('Ctrl Pts',(0.750785745543687,-0.232861760990032,
0.631684198665439));
#5470=CARTESIAN_POINT('Ctrl Pts',(0.763642258217232,-0.224161999508995,
0.615966552324775));
#5471=CARTESIAN_POINT('Ctrl Pts',(0.78555112003688,-0.203463743702801,0.587792702767295));
#5472=CARTESIAN_POINT('Ctrl Pts',(0.795684265985088,-0.190326085855194,
0.573915184558108));
#5473=CARTESIAN_POINT('Ctrl Pts',(0.813159949759,-0.15976606450048,0.548874290046456));
#5474=CARTESIAN_POINT('Ctrl Pts',(0.820511285096538,-0.142345102874864,
0.537715343527944));
#5475=CARTESIAN_POINT('Ctrl Pts',(0.833661031856294,-0.099930567888331,
0.517157748491653));
#5476=CARTESIAN_POINT('Ctrl Pts',(0.838633903678357,-0.0740444353928835,
0.508899795931835));
#5477=CARTESIAN_POINT('Ctrl Pts',(0.841298510752801,-0.0476299999999999,
0.504455939115715));
#5478=CARTESIAN_POINT('',(0.528110872004958,-0.04763,0.871530771444223));
#5479=CARTESIAN_POINT('Origin',(0.707106781186547,-0.04763,0.707106781186548));
#5480=CARTESIAN_POINT('',(0.871530771444223,-0.04763,0.528110872004959));
#5481=CARTESIAN_POINT('Ctrl Pts',(0.871530771444223,-0.0476300000000001,
0.528110872004958));
#5482=CARTESIAN_POINT('Ctrl Pts',(0.87014664509073,-0.0609922781173483,
0.530395067942936));
#5483=CARTESIAN_POINT('Ctrl Pts',(0.868149331745851,-0.0742967091364493,
0.533674141594226));
#5484=CARTESIAN_POINT('Ctrl Pts',(0.85981294420286,-0.115492077056649,0.54708917182331));
#5485=CARTESIAN_POINT('Ctrl Pts',(0.850993704737257,-0.141695629206859,
0.560922177770136));
#5486=CARTESIAN_POINT('Ctrl Pts',(0.830754510485543,-0.181890537957859,
0.590422647829571));
#5487=CARTESIAN_POINT('Ctrl Pts',(0.816896541396381,-0.201072148666545,
0.609616703125488));
#5488=CARTESIAN_POINT('Ctrl Pts',(0.792310597819928,-0.223955109275652,
0.641117951819998));
#5489=CARTESIAN_POINT('Ctrl Pts',(0.779109323683612,-0.232742381310829,
0.657208095763053));
#5490=CARTESIAN_POINT('Ctrl Pts',(0.750552691816206,-0.244234834628584,
0.68964083160521));
#5491=CARTESIAN_POINT('Ctrl Pts',(0.735185187071673,-0.246942143572133,
0.705971972091755));
#5492=CARTESIAN_POINT('Ctrl Pts',(0.705971972091754,-0.246942143572133,
0.735185187071673));
#5493=CARTESIAN_POINT('Ctrl Pts',(0.689640831605209,-0.244234834628584,
0.750552691816206));
#5494=CARTESIAN_POINT('Ctrl Pts',(0.657208095763052,-0.232742381310829,
0.779109323683612));
#5495=CARTESIAN_POINT('Ctrl Pts',(0.641117951819998,-0.223955109275652,
0.792310597819928));
#5496=CARTESIAN_POINT('Ctrl Pts',(0.609616703125487,-0.201072148666545,
0.816896541396382));
#5497=CARTESIAN_POINT('Ctrl Pts',(0.590422647829571,-0.181890537957858,
0.830754510485544));
#5498=CARTESIAN_POINT('Ctrl Pts',(0.560922177770135,-0.141695629206858,
0.850993704737257));
#5499=CARTESIAN_POINT('Ctrl Pts',(0.547089171823309,-0.115492077056649,
0.859812944202861));
#5500=CARTESIAN_POINT('Ctrl Pts',(0.533674141594226,-0.0742967091364491,
0.868149331745852));
#5501=CARTESIAN_POINT('Ctrl Pts',(0.530395067942936,-0.0609922781173483,
0.870146645090731));
#5502=CARTESIAN_POINT('Ctrl Pts',(0.528110872004958,-0.0476300000000001,
0.871530771444223));
#5503=CARTESIAN_POINT('Origin',(0.707106781186547,-0.04763,0.707106781186548));
#5504=CARTESIAN_POINT('Origin',(0.,-0.166705,0.));
#5505=CARTESIAN_POINT('',(0.242834539687906,-0.04763,0.989696097314));
#5506=CARTESIAN_POINT('Origin',(0.,-0.04763,0.));
#5507=CARTESIAN_POINT('',(-0.242834539687907,-0.04763,0.989696097314));
#5508=CARTESIAN_POINT('Ctrl Pts',(0.242834539687906,-0.04763,0.989696097314));
#5509=CARTESIAN_POINT('Ctrl Pts',(0.24024064412003,-0.0609922781173483,
0.990332542620729));
#5510=CARTESIAN_POINT('Ctrl Pts',(0.236509675094874,-0.0742967091364492,
0.991238884025248));
#5511=CARTESIAN_POINT('Ctrl Pts',(0.221129100087819,-0.115492077056649,
0.994830026707808));
#5512=CARTESIAN_POINT('Ctrl Pts',(0.205111543747588,-0.141695629206859,
0.998375294985966));
#5513=CARTESIAN_POINT('Ctrl Pts',(0.169940289819232,-0.181890537957859,
1.00492400591205));
#5514=CARTESIAN_POINT('Ctrl Pts',(0.1465689792446,-0.201072148666545,1.00869718865384));
#5515=CARTESIAN_POINT('Ctrl Pts',(0.106909345252087,-0.223955109275652,
1.01358704779679));
#5516=CARTESIAN_POINT('Ctrl Pts',(0.0861971848975941,-0.232742381310829,
1.0156297872271));
#5517=CARTESIAN_POINT('Ctrl Pts',(0.0430711894098822,-0.244234834628584,
1.01837060663223));
#5518=CARTESIAN_POINT('Ctrl Pts',(0.0206568624125605,-0.246942143572133,
1.019052));
#5519=CARTESIAN_POINT('Ctrl Pts',(-0.0206568624125608,-0.246942143572133,
1.019052));
#5520=CARTESIAN_POINT('Ctrl Pts',(-0.0430711894098825,-0.244234834628584,
1.01837060663223));
#5521=CARTESIAN_POINT('Ctrl Pts',(-0.0861971848975943,-0.232742381310829,
1.0156297872271));
#5522=CARTESIAN_POINT('Ctrl Pts',(-0.106909345252088,-0.223955109275652,
1.01358704779679));
#5523=CARTESIAN_POINT('Ctrl Pts',(-0.1465689792446,-0.201072148666545,1.00869718865384));
#5524=CARTESIAN_POINT('Ctrl Pts',(-0.169940289819232,-0.181890537957859,
1.00492400591205));
#5525=CARTESIAN_POINT('Ctrl Pts',(-0.205111543747588,-0.141695629206859,
0.998375294985966));
#5526=CARTESIAN_POINT('Ctrl Pts',(-0.221129100087819,-0.115492077056649,
0.994830026707808));
#5527=CARTESIAN_POINT('Ctrl Pts',(-0.236509675094875,-0.0742967091364493,
0.991238884025248));
#5528=CARTESIAN_POINT('Ctrl Pts',(-0.24024064412003,-0.0609922781173483,
0.990332542620729));
#5529=CARTESIAN_POINT('Ctrl Pts',(-0.242834539687907,-0.04763,0.989696097314));
#5530=CARTESIAN_POINT('',(-0.528110872004959,-0.04763,0.871530771444223));
#5531=CARTESIAN_POINT('Origin',(0.,-0.04763,0.));
#5532=CARTESIAN_POINT('',(-0.871530771444223,-0.04763,0.528110872004958));
#5533=CARTESIAN_POINT('Ctrl Pts',(-0.528110872004958,-0.0476300000000001,
0.871530771444223));
#5534=CARTESIAN_POINT('Ctrl Pts',(-0.530395067942936,-0.0609922781173484,
0.87014664509073));
#5535=CARTESIAN_POINT('Ctrl Pts',(-0.533674141594226,-0.0742967091364493,
0.868149331745851));
#5536=CARTESIAN_POINT('Ctrl Pts',(-0.54708917182331,-0.115492077056649,
0.85981294420286));
#5537=CARTESIAN_POINT('Ctrl Pts',(-0.560922177770136,-0.141695629206859,
0.850993704737257));
#5538=CARTESIAN_POINT('Ctrl Pts',(-0.590422647829571,-0.181890537957859,
0.830754510485543));
#5539=CARTESIAN_POINT('Ctrl Pts',(-0.609616703125488,-0.201072148666545,
0.816896541396381));
#5540=CARTESIAN_POINT('Ctrl Pts',(-0.641117951819998,-0.223955109275652,
0.792310597819928));
#5541=CARTESIAN_POINT('Ctrl Pts',(-0.657208095763053,-0.232742381310829,
0.779109323683611));
#5542=CARTESIAN_POINT('Ctrl Pts',(-0.68964083160521,-0.244234834628584,
0.750552691816205));
#5543=CARTESIAN_POINT('Ctrl Pts',(-0.705971972091755,-0.246942143572133,
0.735185187071673));
#5544=CARTESIAN_POINT('Ctrl Pts',(-0.735185187071673,-0.246942143572133,
0.705971972091754));
#5545=CARTESIAN_POINT('Ctrl Pts',(-0.750552691816206,-0.244234834628584,
0.689640831605209));
#5546=CARTESIAN_POINT('Ctrl Pts',(-0.779109323683612,-0.232742381310829,
0.657208095763052));
#5547=CARTESIAN_POINT('Ctrl Pts',(-0.792310597819928,-0.223955109275652,
0.641117951819998));
#5548=CARTESIAN_POINT('Ctrl Pts',(-0.816896541396382,-0.201072148666545,
0.609616703125487));
#5549=CARTESIAN_POINT('Ctrl Pts',(-0.830754510485544,-0.181890537957858,
0.590422647829571));
#5550=CARTESIAN_POINT('Ctrl Pts',(-0.850993704737257,-0.141695629206858,
0.560922177770135));
#5551=CARTESIAN_POINT('Ctrl Pts',(-0.859812944202861,-0.115492077056649,
0.547089171823309));
#5552=CARTESIAN_POINT('Ctrl Pts',(-0.868149331745852,-0.0742967091364491,
0.533674141594226));
#5553=CARTESIAN_POINT('Ctrl Pts',(-0.870146645090731,-0.0609922781173483,
0.530395067942936));
#5554=CARTESIAN_POINT('Ctrl Pts',(-0.871530771444223,-0.04763,0.528110872004958));
#5555=CARTESIAN_POINT('',(-0.989696097314,-0.04763,0.242834539687906));
#5556=CARTESIAN_POINT('Origin',(0.,-0.04763,0.));
#5557=CARTESIAN_POINT('',(-1.019052,-0.246942143572133,1.248489836334E-16));
#5558=CARTESIAN_POINT('Ctrl Pts',(-0.989696097314,-0.04763,0.242834539687906));
#5559=CARTESIAN_POINT('Ctrl Pts',(-0.990332542620729,-0.0609922781173483,
0.24024064412003));
#5560=CARTESIAN_POINT('Ctrl Pts',(-0.991238884025248,-0.0742967091364492,
0.236509675094874));
#5561=CARTESIAN_POINT('Ctrl Pts',(-0.994830026707808,-0.115492077056649,
0.221129100087819));
#5562=CARTESIAN_POINT('Ctrl Pts',(-0.998375294985966,-0.141695629206859,
0.205111543747588));
#5563=CARTESIAN_POINT('Ctrl Pts',(-1.00492400591205,-0.181890537957859,
0.169940289819232));
#5564=CARTESIAN_POINT('Ctrl Pts',(-1.00869718865384,-0.201072148666545,
0.1465689792446));
#5565=CARTESIAN_POINT('Ctrl Pts',(-1.01358704779679,-0.223955109275652,
0.106909345252088));
#5566=CARTESIAN_POINT('Ctrl Pts',(-1.0156297872271,-0.232742381310829,0.0861971848975944));
#5567=CARTESIAN_POINT('Ctrl Pts',(-1.01837060663223,-0.244234834628584,
0.0430711894098825));
#5568=CARTESIAN_POINT('Ctrl Pts',(-1.019052,-0.246942143572133,0.0206568624125608));
#5569=CARTESIAN_POINT('Ctrl Pts',(-1.019052,-0.246942143572133,1.2490009027033E-16));
#5570=CARTESIAN_POINT('',(-1.019052,-0.28578,1.24797876996471E-16));
#5571=CARTESIAN_POINT('',(-1.019052,-0.166705,1.24797876996471E-16));
#5572=CARTESIAN_POINT('Origin',(0.,-0.28578,0.));
#5573=CARTESIAN_POINT('',(-0.989696097314,-0.04763,-0.242834539687906));
#5574=CARTESIAN_POINT('Ctrl Pts',(-1.019052,-0.246942143572133,1.2490009027033E-16));
#5575=CARTESIAN_POINT('Ctrl Pts',(-1.019052,-0.246942143572133,-0.0206568624125605));
#5576=CARTESIAN_POINT('Ctrl Pts',(-1.01837060663223,-0.244234834628584,
-0.0430711894098822));
#5577=CARTESIAN_POINT('Ctrl Pts',(-1.0156297872271,-0.232742381310829,-0.0861971848975941));
#5578=CARTESIAN_POINT('Ctrl Pts',(-1.01358704779679,-0.223955109275652,
-0.106909345252087));
#5579=CARTESIAN_POINT('Ctrl Pts',(-1.00869718865384,-0.201072148666546,
-0.1465689792446));
#5580=CARTESIAN_POINT('Ctrl Pts',(-1.00492400591205,-0.181890537957859,
-0.169940289819232));
#5581=CARTESIAN_POINT('Ctrl Pts',(-0.998375294985966,-0.141695629206859,
-0.205111543747588));
#5582=CARTESIAN_POINT('Ctrl Pts',(-0.994830026707808,-0.11549207705665,
-0.221129100087819));
#5583=CARTESIAN_POINT('Ctrl Pts',(-0.991238884025248,-0.0742967091364495,
-0.236509675094874));
#5584=CARTESIAN_POINT('Ctrl Pts',(-0.990332542620729,-0.0609922781173484,
-0.24024064412003));
#5585=CARTESIAN_POINT('Ctrl Pts',(-0.989696097314,-0.0476300000000001,-0.242834539687907));
#5586=CARTESIAN_POINT('',(-0.871530771444223,-0.04763,-0.528110872004958));
#5587=CARTESIAN_POINT('Origin',(0.,-0.04763,0.));
#5588=CARTESIAN_POINT('',(-0.528110872004958,-0.04763,-0.871530771444223));
#5589=CARTESIAN_POINT('Ctrl Pts',(-0.871530771444223,-0.0476300000000001,
-0.528110872004958));
#5590=CARTESIAN_POINT('Ctrl Pts',(-0.87014664509073,-0.0609922781173484,
-0.530395067942936));
#5591=CARTESIAN_POINT('Ctrl Pts',(-0.868149331745851,-0.0742967091364494,
-0.533674141594226));
#5592=CARTESIAN_POINT('Ctrl Pts',(-0.85981294420286,-0.115492077056649,
-0.54708917182331));
#5593=CARTESIAN_POINT('Ctrl Pts',(-0.850993704737257,-0.141695629206859,
-0.560922177770136));
#5594=CARTESIAN_POINT('Ctrl Pts',(-0.830754510485543,-0.181890537957859,
-0.590422647829571));
#5595=CARTESIAN_POINT('Ctrl Pts',(-0.816896541396381,-0.201072148666546,
-0.609616703125488));
#5596=CARTESIAN_POINT('Ctrl Pts',(-0.792310597819928,-0.223955109275652,
-0.641117951819999));
#5597=CARTESIAN_POINT('Ctrl Pts',(-0.779109323683611,-0.232742381310829,
-0.657208095763053));
#5598=CARTESIAN_POINT('Ctrl Pts',(-0.750552691816205,-0.244234834628584,
-0.68964083160521));
#5599=CARTESIAN_POINT('Ctrl Pts',(-0.735185187071673,-0.246942143572133,
-0.705971972091755));
#5600=CARTESIAN_POINT('Ctrl Pts',(-0.705971972091754,-0.246942143572133,
-0.735185187071673));
#5601=CARTESIAN_POINT('Ctrl Pts',(-0.68964083160521,-0.244234834628584,
-0.750552691816206));
#5602=CARTESIAN_POINT('Ctrl Pts',(-0.657208095763052,-0.232742381310829,
-0.779109323683612));
#5603=CARTESIAN_POINT('Ctrl Pts',(-0.641117951819998,-0.223955109275652,
-0.792310597819928));
#5604=CARTESIAN_POINT('Ctrl Pts',(-0.609616703125488,-0.201072148666545,
-0.816896541396381));
#5605=CARTESIAN_POINT('Ctrl Pts',(-0.590422647829571,-0.181890537957859,
-0.830754510485543));
#5606=CARTESIAN_POINT('Ctrl Pts',(-0.560922177770136,-0.141695629206859,
-0.850993704737257));
#5607=CARTESIAN_POINT('Ctrl Pts',(-0.54708917182331,-0.115492077056649,
-0.85981294420286));
#5608=CARTESIAN_POINT('Ctrl Pts',(-0.533674141594226,-0.0742967091364494,
-0.868149331745852));
#5609=CARTESIAN_POINT('Ctrl Pts',(-0.530395067942936,-0.0609922781173484,
-0.870146645090731));
#5610=CARTESIAN_POINT('Ctrl Pts',(-0.528110872004958,-0.0476300000000001,
-0.871530771444223));
#5611=CARTESIAN_POINT('',(-0.242834539687906,-0.04763,-0.989696097314));
#5612=CARTESIAN_POINT('Origin',(0.,-0.04763,0.));
#5613=CARTESIAN_POINT('',(0.242834539687906,-0.04763,-0.989696097314));
#5614=CARTESIAN_POINT('Ctrl Pts',(-0.242834539687907,-0.04763,-0.989696097314));
#5615=CARTESIAN_POINT('Ctrl Pts',(-0.24024064412003,-0.0609922781173483,
-0.990332542620729));
#5616=CARTESIAN_POINT('Ctrl Pts',(-0.236509675094874,-0.0742967091364493,
-0.991238884025248));
#5617=CARTESIAN_POINT('Ctrl Pts',(-0.221129100087819,-0.115492077056649,
-0.994830026707808));
#5618=CARTESIAN_POINT('Ctrl Pts',(-0.205111543747588,-0.141695629206859,
-0.998375294985966));
#5619=CARTESIAN_POINT('Ctrl Pts',(-0.169940289819232,-0.181890537957859,
-1.00492400591205));
#5620=CARTESIAN_POINT('Ctrl Pts',(-0.1465689792446,-0.201072148666545,-1.00869718865384));
#5621=CARTESIAN_POINT('Ctrl Pts',(-0.106909345252087,-0.223955109275652,
-1.01358704779679));
#5622=CARTESIAN_POINT('Ctrl Pts',(-0.0861971848975942,-0.232742381310829,
-1.0156297872271));
#5623=CARTESIAN_POINT('Ctrl Pts',(-0.0430711894098823,-0.244234834628584,
-1.01837060663223));
#5624=CARTESIAN_POINT('Ctrl Pts',(-0.0206568624125606,-0.246942143572133,
-1.019052));
#5625=CARTESIAN_POINT('Ctrl Pts',(0.0206568624125607,-0.246942143572133,
-1.019052));
#5626=CARTESIAN_POINT('Ctrl Pts',(0.0430711894098824,-0.244234834628584,
-1.01837060663223));
#5627=CARTESIAN_POINT('Ctrl Pts',(0.0861971848975943,-0.232742381310829,
-1.0156297872271));
#5628=CARTESIAN_POINT('Ctrl Pts',(0.106909345252088,-0.223955109275652,
-1.01358704779679));
#5629=CARTESIAN_POINT('Ctrl Pts',(0.1465689792446,-0.201072148666545,-1.00869718865384));
#5630=CARTESIAN_POINT('Ctrl Pts',(0.169940289819232,-0.181890537957859,
-1.00492400591205));
#5631=CARTESIAN_POINT('Ctrl Pts',(0.205111543747588,-0.141695629206859,
-0.998375294985966));
#5632=CARTESIAN_POINT('Ctrl Pts',(0.221129100087819,-0.115492077056649,
-0.994830026707808));
#5633=CARTESIAN_POINT('Ctrl Pts',(0.236509675094874,-0.0742967091364493,
-0.991238884025248));
#5634=CARTESIAN_POINT('Ctrl Pts',(0.24024064412003,-0.0609922781173484,
-0.990332542620729));
#5635=CARTESIAN_POINT('Ctrl Pts',(0.242834539687907,-0.04763,-0.989696097314));
#5636=CARTESIAN_POINT('',(0.528110872004958,-0.04763,-0.871530771444223));
#5637=CARTESIAN_POINT('Origin',(0.,-0.04763,0.));
#5638=CARTESIAN_POINT('',(0.871530771444223,-0.04763,-0.528110872004958));
#5639=CARTESIAN_POINT('Ctrl Pts',(0.528110872004958,-0.0476300000000001,
-0.871530771444223));
#5640=CARTESIAN_POINT('Ctrl Pts',(0.530395067942936,-0.0609922781173484,
-0.870146645090731));
#5641=CARTESIAN_POINT('Ctrl Pts',(0.533674141594226,-0.0742967091364493,
-0.868149331745851));
#5642=CARTESIAN_POINT('Ctrl Pts',(0.54708917182331,-0.115492077056649,-0.85981294420286));
#5643=CARTESIAN_POINT('Ctrl Pts',(0.560922177770136,-0.141695629206859,
-0.850993704737257));
#5644=CARTESIAN_POINT('Ctrl Pts',(0.590422647829571,-0.181890537957859,
-0.830754510485543));
#5645=CARTESIAN_POINT('Ctrl Pts',(0.609616703125488,-0.201072148666545,
-0.816896541396381));
#5646=CARTESIAN_POINT('Ctrl Pts',(0.641117951819998,-0.223955109275652,
-0.792310597819928));
#5647=CARTESIAN_POINT('Ctrl Pts',(0.657208095763053,-0.232742381310829,
-0.779109323683612));
#5648=CARTESIAN_POINT('Ctrl Pts',(0.68964083160521,-0.244234834628584,-0.750552691816206));
#5649=CARTESIAN_POINT('Ctrl Pts',(0.705971972091755,-0.246942143572133,
-0.735185187071673));
#5650=CARTESIAN_POINT('Ctrl Pts',(0.735185187071673,-0.246942143572133,
-0.705971972091754));
#5651=CARTESIAN_POINT('Ctrl Pts',(0.750552691816206,-0.244234834628584,
-0.68964083160521));
#5652=CARTESIAN_POINT('Ctrl Pts',(0.779109323683612,-0.232742381310829,
-0.657208095763053));
#5653=CARTESIAN_POINT('Ctrl Pts',(0.792310597819928,-0.223955109275652,
-0.641117951819998));
#5654=CARTESIAN_POINT('Ctrl Pts',(0.816896541396381,-0.201072148666545,
-0.609616703125488));
#5655=CARTESIAN_POINT('Ctrl Pts',(0.830754510485543,-0.181890537957859,
-0.590422647829571));
#5656=CARTESIAN_POINT('Ctrl Pts',(0.850993704737257,-0.141695629206859,
-0.560922177770136));
#5657=CARTESIAN_POINT('Ctrl Pts',(0.85981294420286,-0.115492077056649,-0.54708917182331));
#5658=CARTESIAN_POINT('Ctrl Pts',(0.868149331745851,-0.0742967091364493,
-0.533674141594226));
#5659=CARTESIAN_POINT('Ctrl Pts',(0.870146645090731,-0.0609922781173484,
-0.530395067942936));
#5660=CARTESIAN_POINT('Ctrl Pts',(0.871530771444223,-0.0476300000000001,
-0.528110872004958));
#5661=CARTESIAN_POINT('',(0.989696097314,-0.04763,-0.242834539687906));
#5662=CARTESIAN_POINT('Origin',(0.,-0.04763,0.));
#5663=CARTESIAN_POINT('',(0.989696097314,-0.04763,0.242834539687906));
#5664=CARTESIAN_POINT('Ctrl Pts',(0.989696097314,-0.04763,-0.242834539687907));
#5665=CARTESIAN_POINT('Ctrl Pts',(0.990332542620729,-0.0609922781173483,
-0.24024064412003));
#5666=CARTESIAN_POINT('Ctrl Pts',(0.991238884025248,-0.0742967091364493,
-0.236509675094874));
#5667=CARTESIAN_POINT('Ctrl Pts',(0.994830026707808,-0.115492077056649,
-0.221129100087819));
#5668=CARTESIAN_POINT('Ctrl Pts',(0.998375294985966,-0.141695629206859,
-0.205111543747588));
#5669=CARTESIAN_POINT('Ctrl Pts',(1.00492400591205,-0.181890537957859,-0.169940289819232));
#5670=CARTESIAN_POINT('Ctrl Pts',(1.00869718865384,-0.201072148666545,-0.1465689792446));
#5671=CARTESIAN_POINT('Ctrl Pts',(1.01358704779679,-0.223955109275652,-0.106909345252087));
#5672=CARTESIAN_POINT('Ctrl Pts',(1.0156297872271,-0.232742381310829,-0.0861971848975942));
#5673=CARTESIAN_POINT('Ctrl Pts',(1.01837060663223,-0.244234834628584,-0.0430711894098823));
#5674=CARTESIAN_POINT('Ctrl Pts',(1.019052,-0.246942143572133,-0.0206568624125607));
#5675=CARTESIAN_POINT('Ctrl Pts',(1.019052,-0.246942143572133,0.0206568624125607));
#5676=CARTESIAN_POINT('Ctrl Pts',(1.01837060663223,-0.244234834628584,0.0430711894098823));
#5677=CARTESIAN_POINT('Ctrl Pts',(1.0156297872271,-0.232742381310829,0.0861971848975942));
#5678=CARTESIAN_POINT('Ctrl Pts',(1.01358704779679,-0.223955109275652,0.106909345252087));
#5679=CARTESIAN_POINT('Ctrl Pts',(1.00869718865384,-0.201072148666545,0.1465689792446));
#5680=CARTESIAN_POINT('Ctrl Pts',(1.00492400591205,-0.181890537957859,0.169940289819232));
#5681=CARTESIAN_POINT('Ctrl Pts',(0.998375294985966,-0.141695629206859,
0.205111543747588));
#5682=CARTESIAN_POINT('Ctrl Pts',(0.994830026707808,-0.115492077056649,
0.221129100087819));
#5683=CARTESIAN_POINT('Ctrl Pts',(0.991238884025248,-0.0742967091364492,
0.236509675094874));
#5684=CARTESIAN_POINT('Ctrl Pts',(0.990332542620729,-0.0609922781173483,
0.24024064412003));
#5685=CARTESIAN_POINT('Ctrl Pts',(0.989696097314,-0.04763,0.242834539687907));
#5686=CARTESIAN_POINT('Origin',(0.,-0.04763,0.));
#5687=CARTESIAN_POINT('Origin',(0.,-0.04763,0.));
#5688=CARTESIAN_POINT('',(0.238183666596899,-0.04763,0.951592097314));
#5689=CARTESIAN_POINT('Origin',(0.,-0.04763,0.));
#5690=CARTESIAN_POINT('Origin',(-1.94289029309402E-16,-0.04763,1.));
#5691=CARTESIAN_POINT('Origin',(-1.94289029309402E-16,0.,1.));
#5692=CARTESIAN_POINT('',(-0.2381836665969,-0.04763,0.951592097314));
#5693=CARTESIAN_POINT('Ctrl Pts',(-0.238183666596899,-0.0476299999999999,
0.951592097314));
#5694=CARTESIAN_POINT('Ctrl Pts',(-0.233157223576062,-0.0740444353928835,
0.952850216871763));
#5695=CARTESIAN_POINT('Ctrl Pts',(-0.223801617934946,-0.0999305678883309,
0.955173119738174));
#5696=CARTESIAN_POINT('Ctrl Pts',(-0.199966927975188,-0.142345102874864,
0.960411259488514));
#5697=CARTESIAN_POINT('Ctrl Pts',(-0.1868781821531,-0.159766064500479,0.963103647174702));
#5698=CARTESIAN_POINT('Ctrl Pts',(-0.15681442133453,-0.190326085855194,
0.968453058988463));
#5699=CARTESIAN_POINT('Ctrl Pts',(-0.139836317888043,-0.203463743702801,
0.971100730005489));
#5700=CARTESIAN_POINT('Ctrl Pts',(-0.104422493053067,-0.224161999508995,
0.975530745318961));
#5701=CARTESIAN_POINT('Ctrl Pts',(-0.0842175114474176,-0.232861760990032,
0.977553872336861));
#5702=CARTESIAN_POINT('Ctrl Pts',(-0.0421062857595701,-0.244251601209411,
0.980270995488453));
#5703=CARTESIAN_POINT('Ctrl Pts',(-0.0201990724523197,-0.246942143572133,
0.980948));
#5704=CARTESIAN_POINT('Ctrl Pts',(0.020199072452319,-0.246942143572133,
0.980948));
#5705=CARTESIAN_POINT('Ctrl Pts',(0.0421062857595694,-0.244251601209411,
0.980270995488454));
#5706=CARTESIAN_POINT('Ctrl Pts',(0.0842175114474169,-0.232861760990032,
0.977553872336861));
#5707=CARTESIAN_POINT('Ctrl Pts',(0.104422493053067,-0.224161999508995,
0.975530745318961));
#5708=CARTESIAN_POINT('Ctrl Pts',(0.139836317888042,-0.203463743702801,
0.971100730005489));
#5709=CARTESIAN_POINT('Ctrl Pts',(0.15681442133453,-0.190326085855194,0.968453058988463));
#5710=CARTESIAN_POINT('Ctrl Pts',(0.1868781821531,-0.15976606450048,0.963103647174702));
#5711=CARTESIAN_POINT('Ctrl Pts',(0.199966927975188,-0.142345102874864,
0.960411259488514));
#5712=CARTESIAN_POINT('Ctrl Pts',(0.223801617934945,-0.0999305678883309,
0.955173119738174));
#5713=CARTESIAN_POINT('Ctrl Pts',(0.233157223576061,-0.0740444353928835,
0.952850216871763));
#5714=CARTESIAN_POINT('Ctrl Pts',(0.238183666596899,-0.0476299999999999,
0.951592097314));
#5715=CARTESIAN_POINT('Origin',(-1.94289029309402E-16,-0.04763,1.));
#5716=CARTESIAN_POINT('Origin',(0.,-0.04763,0.));
#5717=CARTESIAN_POINT('',(-0.504455939115715,-0.04763,0.841298510752802));
#5718=CARTESIAN_POINT('Origin',(0.,-0.04763,0.));
#5719=CARTESIAN_POINT('Origin',(-0.707106781186548,-0.04763,0.707106781186547));
#5720=CARTESIAN_POINT('Origin',(-0.707106781186548,0.,0.707106781186547));
#5721=CARTESIAN_POINT('',(-0.841298510752802,-0.04763,0.504455939115715));
#5722=CARTESIAN_POINT('Ctrl Pts',(-0.841298510752802,-0.04763,0.504455939115715));
#5723=CARTESIAN_POINT('Ctrl Pts',(-0.838633903678357,-0.0740444353928835,
0.508899795931835));
#5724=CARTESIAN_POINT('Ctrl Pts',(-0.833661031856294,-0.0999305678883309,
0.517157748491652));
#5725=CARTESIAN_POINT('Ctrl Pts',(-0.820511285096538,-0.142345102874864,
0.537715343527944));
#5726=CARTESIAN_POINT('Ctrl Pts',(-0.813159949759,-0.159766064500479,0.548874290046456));
#5727=CARTESIAN_POINT('Ctrl Pts',(-0.795684265985089,-0.190326085855194,
0.573915184558107));
#5728=CARTESIAN_POINT('Ctrl Pts',(-0.78555112003688,-0.203463743702801,
0.587792702767295));
#5729=CARTESIAN_POINT('Ctrl Pts',(-0.763642258217233,-0.224161999508995,
0.615966552324775));
#5730=CARTESIAN_POINT('Ctrl Pts',(-0.750785745543687,-0.232861760990032,
0.631684198665438));
#5731=CARTESIAN_POINT('Ctrl Pts',(-0.722929908501543,-0.244251601209411,
0.663382628119203));
#5732=CARTESIAN_POINT('Ctrl Pts',(-0.707917883896095,-0.246942143572133,
0.679352081686668));
#5733=CARTESIAN_POINT('Ctrl Pts',(-0.679352081686668,-0.246942143572133,
0.707917883896095));
#5734=CARTESIAN_POINT('Ctrl Pts',(-0.663382628119203,-0.244251601209411,
0.722929908501544));
#5735=CARTESIAN_POINT('Ctrl Pts',(-0.631684198665438,-0.232861760990031,
0.750785745543687));
#5736=CARTESIAN_POINT('Ctrl Pts',(-0.615966552324775,-0.224161999508995,
0.763642258217233));
#5737=CARTESIAN_POINT('Ctrl Pts',(-0.587792702767295,-0.203463743702801,
0.78555112003688));
#5738=CARTESIAN_POINT('Ctrl Pts',(-0.573915184558107,-0.190326085855194,
0.795684265985088));
#5739=CARTESIAN_POINT('Ctrl Pts',(-0.548874290046456,-0.159766064500479,
0.813159949759));
#5740=CARTESIAN_POINT('Ctrl Pts',(-0.537715343527944,-0.142345102874864,
0.820511285096538));
#5741=CARTESIAN_POINT('Ctrl Pts',(-0.517157748491652,-0.0999305678883309,
0.833661031856294));
#5742=CARTESIAN_POINT('Ctrl Pts',(-0.508899795931835,-0.0740444353928835,
0.838633903678357));
#5743=CARTESIAN_POINT('Ctrl Pts',(-0.504455939115716,-0.04763,0.841298510752801));
#5744=CARTESIAN_POINT('Origin',(-0.707106781186548,-0.04763,0.707106781186547));
#5745=CARTESIAN_POINT('Origin',(0.,-0.04763,0.));
#5746=CARTESIAN_POINT('',(-0.951592097314,-0.04763,0.238183666596899));
#5747=CARTESIAN_POINT('Origin',(0.,-0.04763,0.));
#5748=CARTESIAN_POINT('Origin',(-1.,-0.04763,-1.11022302462516E-16));
#5749=CARTESIAN_POINT('Origin',(-1.,0.,-1.11022302462516E-16));
#5750=CARTESIAN_POINT('',(-0.951592097314,-0.04763,-0.2381836665969));
#5751=CARTESIAN_POINT('',(-0.980948,-0.246942143572133,1.08514323328844E-18));
#5752=CARTESIAN_POINT('Ctrl Pts',(-0.951592097314,-0.04763,-0.238183666596899));
#5753=CARTESIAN_POINT('Ctrl Pts',(-0.952850216871763,-0.0740444353928835,
-0.233157223576062));
#5754=CARTESIAN_POINT('Ctrl Pts',(-0.955173119738174,-0.0999305678883309,
-0.223801617934946));
#5755=CARTESIAN_POINT('Ctrl Pts',(-0.960411259488514,-0.142345102874864,
-0.199966927975188));
#5756=CARTESIAN_POINT('Ctrl Pts',(-0.963103647174702,-0.159766064500479,
-0.1868781821531));
#5757=CARTESIAN_POINT('Ctrl Pts',(-0.968453058988463,-0.190326085855194,
-0.15681442133453));
#5758=CARTESIAN_POINT('Ctrl Pts',(-0.971100730005489,-0.203463743702801,
-0.139836317888043));
#5759=CARTESIAN_POINT('Ctrl Pts',(-0.975530745318961,-0.224161999508995,
-0.104422493053067));
#5760=CARTESIAN_POINT('Ctrl Pts',(-0.977553872336861,-0.232861760990032,
-0.0842175114474175));
#5761=CARTESIAN_POINT('Ctrl Pts',(-0.980270995488453,-0.244251601209411,
-0.0421062857595699));
#5762=CARTESIAN_POINT('Ctrl Pts',(-0.980948,-0.246942143572133,-0.0201990724523195));
#5763=CARTESIAN_POINT('Ctrl Pts',(-0.980948,-0.246942143572133,-1.17961196366423E-16));
#5764=CARTESIAN_POINT('Origin',(-1.,-0.04763,-1.11022302462516E-16));
#5765=CARTESIAN_POINT('Ctrl Pts',(-0.980948,-0.246942143572133,-1.17961196366423E-16));
#5766=CARTESIAN_POINT('Ctrl Pts',(-0.980948,-0.246942143572133,0.0201990724523192));
#5767=CARTESIAN_POINT('Ctrl Pts',(-0.980270995488453,-0.244251601209411,
0.0421062857595695));
#5768=CARTESIAN_POINT('Ctrl Pts',(-0.977553872336861,-0.232861760990032,
0.0842175114474169));
#5769=CARTESIAN_POINT('Ctrl Pts',(-0.975530745318961,-0.224161999508995,
0.104422493053066));
#5770=CARTESIAN_POINT('Ctrl Pts',(-0.971100730005489,-0.203463743702801,
0.139836317888042));
#5771=CARTESIAN_POINT('Ctrl Pts',(-0.968453058988463,-0.190326085855194,
0.15681442133453));
#5772=CARTESIAN_POINT('Ctrl Pts',(-0.963103647174702,-0.15976606450048,
0.1868781821531));
#5773=CARTESIAN_POINT('Ctrl Pts',(-0.960411259488514,-0.142345102874864,
0.199966927975188));
#5774=CARTESIAN_POINT('Ctrl Pts',(-0.955173119738174,-0.099930567888331,
0.223801617934945));
#5775=CARTESIAN_POINT('Ctrl Pts',(-0.952850216871763,-0.0740444353928835,
0.233157223576061));
#5776=CARTESIAN_POINT('Ctrl Pts',(-0.951592097314,-0.04763,0.238183666596899));
#5777=CARTESIAN_POINT('Origin',(0.,-0.04763,0.));
#5778=CARTESIAN_POINT('',(-0.841298510752802,-0.04763,-0.504455939115715));
#5779=CARTESIAN_POINT('Origin',(0.,-0.04763,0.));
#5780=CARTESIAN_POINT('Origin',(-0.707106781186547,-0.04763,-0.707106781186548));
#5781=CARTESIAN_POINT('Origin',(-0.707106781186547,0.,-0.707106781186548));
#5782=CARTESIAN_POINT('',(-0.504455939115715,-0.04763,-0.841298510752802));
#5783=CARTESIAN_POINT('Ctrl Pts',(-0.504455939115715,-0.04763,-0.841298510752802));
#5784=CARTESIAN_POINT('Ctrl Pts',(-0.508899795931835,-0.0740444353928835,
-0.838633903678357));
#5785=CARTESIAN_POINT('Ctrl Pts',(-0.517157748491652,-0.0999305678883309,
-0.833661031856294));
#5786=CARTESIAN_POINT('Ctrl Pts',(-0.537715343527944,-0.142345102874864,
-0.820511285096538));
#5787=CARTESIAN_POINT('Ctrl Pts',(-0.548874290046456,-0.159766064500479,
-0.813159949759));
#5788=CARTESIAN_POINT('Ctrl Pts',(-0.573915184558107,-0.190326085855194,
-0.795684265985089));
#5789=CARTESIAN_POINT('Ctrl Pts',(-0.587792702767295,-0.203463743702801,
-0.78555112003688));
#5790=CARTESIAN_POINT('Ctrl Pts',(-0.615966552324775,-0.224161999508995,
-0.763642258217233));
#5791=CARTESIAN_POINT('Ctrl Pts',(-0.631684198665438,-0.232861760990032,
-0.750785745543687));
#5792=CARTESIAN_POINT('Ctrl Pts',(-0.663382628119203,-0.244251601209411,
-0.722929908501543));
#5793=CARTESIAN_POINT('Ctrl Pts',(-0.679352081686668,-0.246942143572133,
-0.707917883896095));
#5794=CARTESIAN_POINT('Ctrl Pts',(-0.707917883896095,-0.246942143572133,
-0.679352081686668));
#5795=CARTESIAN_POINT('Ctrl Pts',(-0.722929908501543,-0.244251601209411,
-0.663382628119203));
#5796=CARTESIAN_POINT('Ctrl Pts',(-0.750785745543687,-0.232861760990032,
-0.631684198665439));
#5797=CARTESIAN_POINT('Ctrl Pts',(-0.763642258217232,-0.224161999508995,
-0.615966552324775));
#5798=CARTESIAN_POINT('Ctrl Pts',(-0.78555112003688,-0.203463743702801,
-0.587792702767295));
#5799=CARTESIAN_POINT('Ctrl Pts',(-0.795684265985088,-0.190326085855194,
-0.573915184558107));
#5800=CARTESIAN_POINT('Ctrl Pts',(-0.813159949759,-0.15976606450048,-0.548874290046456));
#5801=CARTESIAN_POINT('Ctrl Pts',(-0.820511285096538,-0.142345102874864,
-0.537715343527944));
#5802=CARTESIAN_POINT('Ctrl Pts',(-0.833661031856294,-0.0999305678883311,
-0.517157748491652));
#5803=CARTESIAN_POINT('Ctrl Pts',(-0.838633903678357,-0.0740444353928836,
-0.508899795931835));
#5804=CARTESIAN_POINT('Ctrl Pts',(-0.841298510752801,-0.04763,-0.504455939115715));
#5805=CARTESIAN_POINT('Origin',(-0.707106781186547,-0.04763,-0.707106781186548));
#5806=CARTESIAN_POINT('Origin',(0.,-0.04763,0.));
#5807=CARTESIAN_POINT('',(-0.238183666596899,-0.04763,-0.951592097314));
#5808=CARTESIAN_POINT('Origin',(0.,-0.04763,0.));
#5809=CARTESIAN_POINT('Origin',(5.55111512312578E-17,-0.04763,-1.));
#5810=CARTESIAN_POINT('Origin',(5.55111512312578E-17,0.,-1.));
#5811=CARTESIAN_POINT('',(0.238183666596899,-0.04763,-0.951592097314));
#5812=CARTESIAN_POINT('Ctrl Pts',(0.238183666596899,-0.04763,-0.951592097314));
#5813=CARTESIAN_POINT('Ctrl Pts',(0.233157223576062,-0.0740444353928835,
-0.952850216871763));
#5814=CARTESIAN_POINT('Ctrl Pts',(0.223801617934946,-0.099930567888331,
-0.955173119738174));
#5815=CARTESIAN_POINT('Ctrl Pts',(0.199966927975188,-0.142345102874864,
-0.960411259488514));
#5816=CARTESIAN_POINT('Ctrl Pts',(0.1868781821531,-0.15976606450048,-0.963103647174702));
#5817=CARTESIAN_POINT('Ctrl Pts',(0.15681442133453,-0.190326085855194,-0.968453058988463));
#5818=CARTESIAN_POINT('Ctrl Pts',(0.139836317888042,-0.203463743702801,
-0.971100730005489));
#5819=CARTESIAN_POINT('Ctrl Pts',(0.104422493053067,-0.224161999508995,
-0.975530745318961));
#5820=CARTESIAN_POINT('Ctrl Pts',(0.0842175114474173,-0.232861760990032,
-0.977553872336861));
#5821=CARTESIAN_POINT('Ctrl Pts',(0.0421062857595698,-0.244251601209411,
-0.980270995488453));
#5822=CARTESIAN_POINT('Ctrl Pts',(0.0201990724523194,-0.246942143572133,
-0.980948));
#5823=CARTESIAN_POINT('Ctrl Pts',(-0.0201990724523193,-0.246942143572133,
-0.980948));
#5824=CARTESIAN_POINT('Ctrl Pts',(-0.0421062857595697,-0.244251601209411,
-0.980270995488453));
#5825=CARTESIAN_POINT('Ctrl Pts',(-0.0842175114474171,-0.232861760990032,
-0.977553872336861));
#5826=CARTESIAN_POINT('Ctrl Pts',(-0.104422493053067,-0.224161999508995,
-0.975530745318961));
#5827=CARTESIAN_POINT('Ctrl Pts',(-0.139836317888042,-0.203463743702801,
-0.971100730005489));
#5828=CARTESIAN_POINT('Ctrl Pts',(-0.15681442133453,-0.190326085855194,
-0.968453058988463));
#5829=CARTESIAN_POINT('Ctrl Pts',(-0.1868781821531,-0.15976606450048,-0.963103647174702));
#5830=CARTESIAN_POINT('Ctrl Pts',(-0.199966927975188,-0.142345102874864,
-0.960411259488514));
#5831=CARTESIAN_POINT('Ctrl Pts',(-0.223801617934945,-0.099930567888331,
-0.955173119738174));
#5832=CARTESIAN_POINT('Ctrl Pts',(-0.233157223576062,-0.0740444353928835,
-0.952850216871763));
#5833=CARTESIAN_POINT('Ctrl Pts',(-0.238183666596899,-0.0476299999999999,
-0.951592097314));
#5834=CARTESIAN_POINT('Origin',(5.55111512312578E-17,-0.04763,-1.));
#5835=CARTESIAN_POINT('Origin',(0.,-0.04763,0.));
#5836=CARTESIAN_POINT('',(0.504455939115715,-0.04763,-0.841298510752802));
#5837=CARTESIAN_POINT('Origin',(0.,-0.04763,0.));
#5838=CARTESIAN_POINT('Origin',(0.707106781186548,-0.04763,-0.707106781186547));
#5839=CARTESIAN_POINT('Origin',(0.707106781186548,0.,-0.707106781186547));
#5840=CARTESIAN_POINT('',(0.841298510752802,-0.04763,-0.504455939115715));
#5841=CARTESIAN_POINT('Ctrl Pts',(0.841298510752802,-0.04763,-0.504455939115715));
#5842=CARTESIAN_POINT('Ctrl Pts',(0.838633903678357,-0.0740444353928835,
-0.508899795931835));
#5843=CARTESIAN_POINT('Ctrl Pts',(0.833661031856294,-0.0999305678883309,
-0.517157748491652));
#5844=CARTESIAN_POINT('Ctrl Pts',(0.820511285096538,-0.142345102874864,
-0.537715343527944));
#5845=CARTESIAN_POINT('Ctrl Pts',(0.813159949759,-0.159766064500479,-0.548874290046456));
#5846=CARTESIAN_POINT('Ctrl Pts',(0.795684265985088,-0.190326085855194,
-0.573915184558107));
#5847=CARTESIAN_POINT('Ctrl Pts',(0.78555112003688,-0.203463743702801,-0.587792702767295));
#5848=CARTESIAN_POINT('Ctrl Pts',(0.763642258217233,-0.224161999508995,
-0.615966552324775));
#5849=CARTESIAN_POINT('Ctrl Pts',(0.750785745543687,-0.232861760990032,
-0.631684198665438));
#5850=CARTESIAN_POINT('Ctrl Pts',(0.722929908501543,-0.244251601209411,
-0.663382628119203));
#5851=CARTESIAN_POINT('Ctrl Pts',(0.707917883896095,-0.246942143572133,
-0.679352081686668));
#5852=CARTESIAN_POINT('Ctrl Pts',(0.679352081686668,-0.246942143572133,
-0.707917883896095));
#5853=CARTESIAN_POINT('Ctrl Pts',(0.663382628119203,-0.244251601209411,
-0.722929908501543));
#5854=CARTESIAN_POINT('Ctrl Pts',(0.631684198665438,-0.232861760990032,
-0.750785745543687));
#5855=CARTESIAN_POINT('Ctrl Pts',(0.615966552324775,-0.224161999508995,
-0.763642258217232));
#5856=CARTESIAN_POINT('Ctrl Pts',(0.587792702767295,-0.203463743702801,
-0.78555112003688));
#5857=CARTESIAN_POINT('Ctrl Pts',(0.573915184558107,-0.190326085855194,
-0.795684265985088));
#5858=CARTESIAN_POINT('Ctrl Pts',(0.548874290046456,-0.159766064500479,
-0.813159949759));
#5859=CARTESIAN_POINT('Ctrl Pts',(0.537715343527944,-0.142345102874864,
-0.820511285096538));
#5860=CARTESIAN_POINT('Ctrl Pts',(0.517157748491652,-0.099930567888331,
-0.833661031856294));
#5861=CARTESIAN_POINT('Ctrl Pts',(0.508899795931835,-0.0740444353928835,
-0.838633903678357));
#5862=CARTESIAN_POINT('Ctrl Pts',(0.504455939115715,-0.04763,-0.841298510752801));
#5863=CARTESIAN_POINT('Origin',(0.707106781186548,-0.04763,-0.707106781186547));
#5864=CARTESIAN_POINT('Origin',(0.,-0.166705,0.));
#5865=CARTESIAN_POINT('',(-0.980948,-0.28578,1.20131482833E-16));
#5866=CARTESIAN_POINT('Origin',(0.,-0.28578,0.));
#5867=CARTESIAN_POINT('',(-0.980948,-0.166705,1.20131482833E-16));
#5868=CARTESIAN_POINT('',(0.951592097314,-0.04763,0.238183666596899));
#5869=CARTESIAN_POINT('Origin',(0.,-0.04763,0.));
#5870=CARTESIAN_POINT('',(0.951592097314,-0.04763,-0.238183666596899));
#5871=CARTESIAN_POINT('Ctrl Pts',(0.951592097314,-0.04763,0.238183666596899));
#5872=CARTESIAN_POINT('Ctrl Pts',(0.952850216871763,-0.0740444353928835,
0.233157223576062));
#5873=CARTESIAN_POINT('Ctrl Pts',(0.955173119738174,-0.099930567888331,
0.223801617934945));
#5874=CARTESIAN_POINT('Ctrl Pts',(0.960411259488514,-0.142345102874864,
0.199966927975188));
#5875=CARTESIAN_POINT('Ctrl Pts',(0.963103647174702,-0.15976606450048,0.1868781821531));
#5876=CARTESIAN_POINT('Ctrl Pts',(0.968453058988463,-0.190326085855194,
0.15681442133453));
#5877=CARTESIAN_POINT('Ctrl Pts',(0.971100730005489,-0.203463743702801,
0.139836317888042));
#5878=CARTESIAN_POINT('Ctrl Pts',(0.975530745318961,-0.224161999508995,
0.104422493053067));
#5879=CARTESIAN_POINT('Ctrl Pts',(0.977553872336861,-0.232861760990032,
0.0842175114474172));
#5880=CARTESIAN_POINT('Ctrl Pts',(0.980270995488453,-0.244251601209411,
0.0421062857595697));
#5881=CARTESIAN_POINT('Ctrl Pts',(0.980948,-0.246942143572133,0.0201990724523194));
#5882=CARTESIAN_POINT('Ctrl Pts',(0.980948,-0.246942143572133,-0.0201990724523194));
#5883=CARTESIAN_POINT('Ctrl Pts',(0.980270995488453,-0.244251601209411,
-0.0421062857595697));
#5884=CARTESIAN_POINT('Ctrl Pts',(0.977553872336861,-0.232861760990032,
-0.0842175114474172));
#5885=CARTESIAN_POINT('Ctrl Pts',(0.975530745318961,-0.224161999508995,
-0.104422493053067));
#5886=CARTESIAN_POINT('Ctrl Pts',(0.971100730005489,-0.203463743702801,
-0.139836317888042));
#5887=CARTESIAN_POINT('Ctrl Pts',(0.968453058988463,-0.190326085855194,
-0.15681442133453));
#5888=CARTESIAN_POINT('Ctrl Pts',(0.963103647174702,-0.15976606450048,-0.1868781821531));
#5889=CARTESIAN_POINT('Ctrl Pts',(0.960411259488514,-0.142345102874864,
-0.199966927975188));
#5890=CARTESIAN_POINT('Ctrl Pts',(0.955173119738174,-0.099930567888331,
-0.223801617934945));
#5891=CARTESIAN_POINT('Ctrl Pts',(0.952850216871763,-0.0740444353928835,
-0.233157223576062));
#5892=CARTESIAN_POINT('Ctrl Pts',(0.951592097314,-0.0476299999999999,-0.238183666596899));
#5893=CARTESIAN_POINT('Origin',(0.,-0.04763,0.));
#5894=CARTESIAN_POINT('Origin',(0.,-0.04763,0.));
#5895=CARTESIAN_POINT('Origin',(1.,-0.04763,0.));
#5896=CARTESIAN_POINT('Origin',(1.,0.,0.));
#5897=CARTESIAN_POINT('Origin',(1.,-0.04763,0.));
#5898=CARTESIAN_POINT('Origin',(0.,-0.28578,0.));
#5899=CARTESIAN_POINT('Origin',(0.,-0.04763,0.));
#5900=CARTESIAN_POINT('',(0.,0.,0.));
#5901=CARTESIAN_POINT('Origin',(1.013815,0.445,0.));
#5902=CARTESIAN_POINT('',(-1.013815,0.445,-1.24156529467757E-16));
#5903=CARTESIAN_POINT('Origin',(0.,0.445,0.));
#5904=CARTESIAN_POINT('',(-0.991185,0.445,-1.21385153761287E-16));
#5905=CARTESIAN_POINT('Origin',(0.,0.445,0.));
#5906=CARTESIAN_POINT('Origin',(0.,0.4075,0.));
#5907=CARTESIAN_POINT('',(-1.013815,0.37,-1.24156529467757E-16));
#5908=CARTESIAN_POINT('Origin',(0.,0.37,0.));
#5909=CARTESIAN_POINT('',(-1.013815,0.4075,-1.24156529467757E-16));
#5910=CARTESIAN_POINT('Origin',(0.991185,0.37,0.));
#5911=CARTESIAN_POINT('',(-0.991185,0.37,-1.21385153761287E-16));
#5912=CARTESIAN_POINT('Origin',(0.,0.37,0.));
#5913=CARTESIAN_POINT('Origin',(0.,0.4075,0.));
#5914=CARTESIAN_POINT('',(-0.991185,0.4075,-1.21385153761287E-16));
#5915=CARTESIAN_POINT('Origin',(1.013815,-0.37,0.));
#5916=CARTESIAN_POINT('',(-1.013815,-0.37,-1.24156529467757E-16));
#5917=CARTESIAN_POINT('Origin',(0.,-0.37,0.));
#5918=CARTESIAN_POINT('',(-0.991185,-0.37,-1.21385153761287E-16));
#5919=CARTESIAN_POINT('Origin',(0.,-0.37,0.));
#5920=CARTESIAN_POINT('Origin',(0.,-0.4075,0.));
#5921=CARTESIAN_POINT('',(-1.013815,-0.445,-1.24156529467757E-16));
#5922=CARTESIAN_POINT('Origin',(0.,-0.445,0.));
#5923=CARTESIAN_POINT('',(-1.013815,-0.4075,-1.24156529467757E-16));
#5924=CARTESIAN_POINT('Origin',(0.991185,-0.445,0.));
#5925=CARTESIAN_POINT('',(-0.991185,-0.445,-1.21385153761287E-16));
#5926=CARTESIAN_POINT('Origin',(0.,-0.445,0.));
#5927=CARTESIAN_POINT('Origin',(0.,-0.4075,0.));
#5928=CARTESIAN_POINT('',(-0.991185,-0.4075,-1.21385153761287E-16));
#5929=CARTESIAN_POINT('',(0.,0.,0.));
#5930=CARTESIAN_POINT('',(0.,0.,0.));
#5931=CARTESIAN_POINT('',(0.,0.,0.));
#5932=CARTESIAN_POINT('',(0.,0.,0.));
#5933=CARTESIAN_POINT('',(0.,0.,0.));
#5934=CARTESIAN_POINT('',(0.,0.,0.));
#5935=CARTESIAN_POINT('',(0.,0.,0.));
#5936=CARTESIAN_POINT('Origin',(-1.9,-0.1,4.5));
#5937=CARTESIAN_POINT('',(-2.065,0.,4.5));
#5938=CARTESIAN_POINT('Origin',(-1.9,0.,4.5));
#5939=CARTESIAN_POINT('',(-2.065,1.2,4.5));
#5940=CARTESIAN_POINT('',(-2.065,-0.1,4.5));
#5941=CARTESIAN_POINT('Origin',(-1.9,1.2,4.5));
#5942=CARTESIAN_POINT('Origin',(1.16341445918999E-16,-0.1,6.4));
#5943=CARTESIAN_POINT('',(-0.165,0.,6.4));
#5944=CARTESIAN_POINT('Origin',(1.16341445918999E-16,0.,6.4));
#5945=CARTESIAN_POINT('',(-0.165,1.2,6.4));
#5946=CARTESIAN_POINT('',(-0.165,-0.1,6.4));
#5947=CARTESIAN_POINT('Origin',(1.16341445918999E-16,1.2,6.4));
#5948=CARTESIAN_POINT('Origin',(1.9,-0.1,4.5));
#5949=CARTESIAN_POINT('',(1.735,0.,4.5));
#5950=CARTESIAN_POINT('Origin',(1.9,0.,4.5));
#5951=CARTESIAN_POINT('',(1.735,1.2,4.5));
#5952=CARTESIAN_POINT('',(1.735,-0.1,4.5));
#5953=CARTESIAN_POINT('Origin',(1.9,1.2,4.5));
#5954=CARTESIAN_POINT('Origin',(-3.49024337756996E-16,-0.1,2.6));
#5955=CARTESIAN_POINT('',(-0.165,0.,2.6));
#5956=CARTESIAN_POINT('Origin',(-3.49024337756996E-16,0.,2.6));
#5957=CARTESIAN_POINT('',(-0.165,1.2,2.6));
#5958=CARTESIAN_POINT('',(-0.165,-0.1,2.6));
#5959=CARTESIAN_POINT('Origin',(-3.49024337756996E-16,1.2,2.6));
#5960=CARTESIAN_POINT('Origin',(0.,0.9,4.5));
#5961=CARTESIAN_POINT('',(-1.2,1.2,4.5));
#5962=CARTESIAN_POINT('Origin',(0.,1.2,4.5));
#5963=CARTESIAN_POINT('',(-1.2,0.9,4.5));
#5964=CARTESIAN_POINT('',(-1.2,0.9,4.5));
#5965=CARTESIAN_POINT('Origin',(0.,0.9,4.5));
#5966=CARTESIAN_POINT('Origin',(0.,0.9,4.5));
#5967=CARTESIAN_POINT('',(-1.5,0.9,4.5));
#5968=CARTESIAN_POINT('Origin',(0.,0.9,4.5));
#5969=CARTESIAN_POINT('Origin',(0.,0.,4.5));
#5970=CARTESIAN_POINT('',(-1.5,0.,4.5));
#5971=CARTESIAN_POINT('',(-1.5,0.,4.5));
#5972=CARTESIAN_POINT('Origin',(0.,0.,4.5));
#5973=CARTESIAN_POINT('Origin',(0.,0.,4.5));
#5974=CARTESIAN_POINT('',(-2.2,1.2,4.5));
#5975=CARTESIAN_POINT('Origin',(0.,1.2,4.5));
#5976=CARTESIAN_POINT('',(-2.2,0.,4.5));
#5977=CARTESIAN_POINT('',(-2.2,0.,4.5));
#5978=CARTESIAN_POINT('Origin',(0.,0.,4.5));
#5979=CARTESIAN_POINT('Origin',(0.,1.2,4.5));
#5980=CARTESIAN_POINT('Origin',(0.,0.,4.5));
#5981=CARTESIAN_POINT('',(0.,0.,0.));
#5982=CARTESIAN_POINT('Origin',(-1.9,28.7,4.5));
#5983=CARTESIAN_POINT('',(-2.065,28.8,4.5));
#5984=CARTESIAN_POINT('Origin',(-1.9,28.8,4.5));
#5985=CARTESIAN_POINT('',(-2.065,30.,4.5));
#5986=CARTESIAN_POINT('',(-2.065,28.7,4.5));
#5987=CARTESIAN_POINT('Origin',(-1.9,30.,4.5));
#5988=CARTESIAN_POINT('Origin',(1.16341445918999E-16,28.7,6.4));
#5989=CARTESIAN_POINT('',(-0.165,28.8,6.4));
#5990=CARTESIAN_POINT('Origin',(1.16341445918999E-16,28.8,6.4));
#5991=CARTESIAN_POINT('',(-0.165,30.,6.4));
#5992=CARTESIAN_POINT('',(-0.165,28.7,6.4));
#5993=CARTESIAN_POINT('Origin',(1.16341445918999E-16,30.,6.4));
#5994=CARTESIAN_POINT('Origin',(1.9,28.7,4.5));
#5995=CARTESIAN_POINT('',(1.735,28.8,4.5));
#5996=CARTESIAN_POINT('Origin',(1.9,28.8,4.5));
#5997=CARTESIAN_POINT('',(1.735,30.,4.5));
#5998=CARTESIAN_POINT('',(1.735,28.7,4.5));
#5999=CARTESIAN_POINT('Origin',(1.9,30.,4.5));
#6000=CARTESIAN_POINT('Origin',(-3.49024337756996E-16,28.7,2.6));
#6001=CARTESIAN_POINT('',(-0.165,28.8,2.6));
#6002=CARTESIAN_POINT('Origin',(-3.49024337756996E-16,28.8,2.6));
#6003=CARTESIAN_POINT('',(-0.165,30.,2.6));
#6004=CARTESIAN_POINT('',(-0.165,28.7,2.6));
#6005=CARTESIAN_POINT('Origin',(-3.49024337756996E-16,30.,2.6));
#6006=CARTESIAN_POINT('Origin',(0.,28.8,4.5));
#6007=CARTESIAN_POINT('',(-1.2,29.1,4.5));
#6008=CARTESIAN_POINT('Origin',(0.,29.1,4.5));
#6009=CARTESIAN_POINT('',(-1.2,28.8,4.5));
#6010=CARTESIAN_POINT('',(-1.2,28.8,4.5));
#6011=CARTESIAN_POINT('Origin',(0.,28.8,4.5));
#6012=CARTESIAN_POINT('Origin',(0.,29.1,4.5));
#6013=CARTESIAN_POINT('',(-1.5,29.1,4.5));
#6014=CARTESIAN_POINT('Origin',(0.,29.1,4.5));
#6015=CARTESIAN_POINT('Origin',(0.,28.8,4.5));
#6016=CARTESIAN_POINT('',(-1.5,30.,4.5));
#6017=CARTESIAN_POINT('Origin',(0.,30.,4.5));
#6018=CARTESIAN_POINT('',(-1.5,28.8,4.5));
#6019=CARTESIAN_POINT('Origin',(0.,28.8,4.5));
#6020=CARTESIAN_POINT('',(-2.2,30.,4.5));
#6021=CARTESIAN_POINT('Origin',(0.,30.,4.5));
#6022=CARTESIAN_POINT('',(-2.2,28.8,4.5));
#6023=CARTESIAN_POINT('',(-2.2,28.8,4.5));
#6024=CARTESIAN_POINT('Origin',(0.,28.8,4.5));
#6025=CARTESIAN_POINT('Origin',(0.,30.,4.5));
#6026=CARTESIAN_POINT('Origin',(0.,28.8,4.5));
#6027=CARTESIAN_POINT('',(0.,0.,0.));
#6028=CARTESIAN_POINT('Origin',(0.,0.,4.5));
#6029=CARTESIAN_POINT('',(-2.2,30.,4.5));
#6030=CARTESIAN_POINT('Origin',(0.,30.,4.5));
#6031=CARTESIAN_POINT('',(-2.2,0.,4.5));
#6032=CARTESIAN_POINT('',(-2.2,0.,4.5));
#6033=CARTESIAN_POINT('Origin',(0.,0.,4.5));
#6034=CARTESIAN_POINT('Origin',(0.,0.,4.5));
#6035=CARTESIAN_POINT('',(-2.5,30.,4.5));
#6036=CARTESIAN_POINT('Origin',(0.,30.,4.5));
#6037=CARTESIAN_POINT('',(-2.5,0.,4.5));
#6038=CARTESIAN_POINT('',(-2.5,0.,4.5));
#6039=CARTESIAN_POINT('Origin',(0.,0.,4.5));
#6040=CARTESIAN_POINT('Origin',(0.,30.,4.5));
#6041=CARTESIAN_POINT('Origin',(0.,0.,4.5));
#6042=CARTESIAN_POINT('',(0.,0.,0.));
#6043=CARTESIAN_POINT('Origin',(-1.9,-0.4,4.5));
#6044=CARTESIAN_POINT('',(-2.125,-0.3,4.5));
#6045=CARTESIAN_POINT('Origin',(-1.9,-0.3,4.5));
#6046=CARTESIAN_POINT('',(-2.125,0.,4.5));
#6047=CARTESIAN_POINT('',(-2.125,-0.4,4.5));
#6048=CARTESIAN_POINT('Origin',(-1.9,0.,4.5));
#6049=CARTESIAN_POINT('Origin',(1.16341445918999E-16,-0.4,6.4));
#6050=CARTESIAN_POINT('',(-0.225,-0.3,6.4));
#6051=CARTESIAN_POINT('Origin',(1.16341445918999E-16,-0.3,6.4));
#6052=CARTESIAN_POINT('',(-0.225,0.,6.4));
#6053=CARTESIAN_POINT('',(-0.225,-0.4,6.4));
#6054=CARTESIAN_POINT('Origin',(1.16341445918999E-16,0.,6.4));
#6055=CARTESIAN_POINT('Origin',(1.9,-0.4,4.5));
#6056=CARTESIAN_POINT('',(1.675,-0.3,4.5));
#6057=CARTESIAN_POINT('Origin',(1.9,-0.3,4.5));
#6058=CARTESIAN_POINT('',(1.675,0.,4.5));
#6059=CARTESIAN_POINT('',(1.675,-0.4,4.5));
#6060=CARTESIAN_POINT('Origin',(1.9,0.,4.5));
#6061=CARTESIAN_POINT('Origin',(-3.49024337756996E-16,-0.4,2.6));
#6062=CARTESIAN_POINT('',(-0.225,-0.3,2.6));
#6063=CARTESIAN_POINT('Origin',(-3.49024337756996E-16,-0.3,2.6));
#6064=CARTESIAN_POINT('',(-0.225,0.,2.6));
#6065=CARTESIAN_POINT('',(-0.225,-0.4,2.6));
#6066=CARTESIAN_POINT('Origin',(-3.49024337756996E-16,0.,2.6));
#6067=CARTESIAN_POINT('Origin',(0.,-0.3,4.5));
#6068=CARTESIAN_POINT('',(-1.2,0.,4.5));
#6069=CARTESIAN_POINT('Origin',(0.,0.,4.5));
#6070=CARTESIAN_POINT('',(-1.2,-0.3,4.5));
#6071=CARTESIAN_POINT('',(-1.2,-0.3,4.5));
#6072=CARTESIAN_POINT('Origin',(0.,-0.3,4.5));
#6073=CARTESIAN_POINT('Origin',(0.,-0.3,4.5));
#6074=CARTESIAN_POINT('',(-2.5,0.,4.5));
#6075=CARTESIAN_POINT('Origin',(0.,0.,4.5));
#6076=CARTESIAN_POINT('',(-2.5,-0.3,4.5));
#6077=CARTESIAN_POINT('',(-2.5,-0.3,4.5));
#6078=CARTESIAN_POINT('Origin',(0.,-0.3,4.5));
#6079=CARTESIAN_POINT('Origin',(0.,0.,4.5));
#6080=CARTESIAN_POINT('Origin',(0.,-0.3,4.5));
#6081=CARTESIAN_POINT('',(0.,0.,0.));
#6082=CARTESIAN_POINT('Origin',(0.3,0.4,0.));
#6083=CARTESIAN_POINT('',(-0.3,0.4,-3.67394039744206E-17));
#6084=CARTESIAN_POINT('Origin',(0.,0.4,0.));
#6085=CARTESIAN_POINT('Origin',(0.,0.375,0.));
#6086=CARTESIAN_POINT('',(-0.35,0.35,-4.28626379701573E-17));
#6087=CARTESIAN_POINT('Origin',(0.,0.35,0.));
#6088=CARTESIAN_POINT('',(-0.325,0.375,-3.9801020972289E-17));
#6089=CARTESIAN_POINT('Origin',(0.,0.19,0.));
#6090=CARTESIAN_POINT('',(-0.35,0.03,-4.28626379701574E-17));
#6091=CARTESIAN_POINT('Origin',(0.,0.03,0.));
#6092=CARTESIAN_POINT('',(-0.35,0.19,-4.28626379701574E-17));
#6093=CARTESIAN_POINT('Origin',(0.,0.0149999999999999,0.));
#6094=CARTESIAN_POINT('',(-0.32,-3.29597460435593E-17,-3.91886975727153E-17));
#6095=CARTESIAN_POINT('Origin',(0.,0.,0.));
#6096=CARTESIAN_POINT('',(-0.335,0.0149999999999999,-4.10256677714363E-17));
#6097=CARTESIAN_POINT('Origin',(0.22,0.,0.));
#6098=CARTESIAN_POINT('',(-0.22,-6.93889390390723E-18,-2.69422295812418E-17));
#6099=CARTESIAN_POINT('Origin',(0.,0.,0.));
#6100=CARTESIAN_POINT('Origin',(0.,-0.02,0.));
#6101=CARTESIAN_POINT('',(-0.1954,-0.0492,2.39295984553393E-17));
#6102=CARTESIAN_POINT('Origin',(0.,-0.0492,0.));
#6103=CARTESIAN_POINT('',(-0.21,-0.02,-2.57175827820944E-17));
#6104=CARTESIAN_POINT('Origin',(0.,-0.8,0.));
#6105=CARTESIAN_POINT('',(-0.1954,-1.5646,2.39295984553393E-17));
#6106=CARTESIAN_POINT('Origin',(0.,-1.5646,0.));
#6107=CARTESIAN_POINT('',(-0.1954,-0.8,-2.39295984553393E-17));
#6108=CARTESIAN_POINT('Origin',(0.,-1.58,0.));
#6109=CARTESIAN_POINT('',(-0.16,-1.6,-1.95943487863577E-17));
#6110=CARTESIAN_POINT('Origin',(0.,-1.6,0.));
#6111=CARTESIAN_POINT('',(-0.18,-1.58,-2.20436423846524E-17));
#6112=CARTESIAN_POINT('Origin',(0.,-1.6,0.));
#6113=CARTESIAN_POINT('Origin',(0.0866025403784439,-0.4,-0.15));
#6114=CARTESIAN_POINT('',(0.173205080756888,-0.4,0.));
#6115=CARTESIAN_POINT('',(0.0866025403784439,-0.4,-0.15));
#6116=CARTESIAN_POINT('',(0.173205080756888,-0.4,0.));
#6117=CARTESIAN_POINT('',(0.0866025403784439,-0.64,-0.15));
#6118=CARTESIAN_POINT('',(0.0866025403784439,-0.4,-0.15));
#6119=CARTESIAN_POINT('',(0.173205080756888,-0.64,0.));
#6120=CARTESIAN_POINT('',(0.173205080756888,-0.64,0.));
#6121=CARTESIAN_POINT('',(0.173205080756888,-0.4,0.));
#6122=CARTESIAN_POINT('Origin',(-0.0866025403784438,-0.4,-0.15));
#6123=CARTESIAN_POINT('',(-0.0866025403784438,-0.4,-0.15));
#6124=CARTESIAN_POINT('',(0.0866025403784439,-0.4,-0.15));
#6125=CARTESIAN_POINT('',(-0.0866025403784438,-0.64,-0.15));
#6126=CARTESIAN_POINT('',(-0.0866025403784438,-0.4,-0.15));
#6127=CARTESIAN_POINT('',(0.0866025403784439,-0.64,-0.15));
#6128=CARTESIAN_POINT('Origin',(-0.173205080756888,-0.4,-2.77555756156289E-17));
#6129=CARTESIAN_POINT('',(-0.173205080756888,-0.4,-2.12115047744981E-17));
#6130=CARTESIAN_POINT('',(-0.0866025403784438,-0.4,-0.15));
#6131=CARTESIAN_POINT('',(-0.173205080756888,-0.64,-2.77555756156289E-17));
#6132=CARTESIAN_POINT('',(-0.173205080756888,-0.4,-2.12115047744981E-17));
#6133=CARTESIAN_POINT('',(-0.0866025403784438,-0.64,-0.15));
#6134=CARTESIAN_POINT('Origin',(-0.0866025403784439,-0.4,0.15));
#6135=CARTESIAN_POINT('',(-0.0866025403784439,-0.4,0.15));
#6136=CARTESIAN_POINT('',(-0.173205080756888,-0.4,-2.12115047744981E-17));
#6137=CARTESIAN_POINT('',(-0.0866025403784439,-0.64,0.15));
#6138=CARTESIAN_POINT('',(-0.0866025403784439,-0.4,0.15));
#6139=CARTESIAN_POINT('',(-0.173205080756888,-0.64,-2.12115047744981E-17));
#6140=CARTESIAN_POINT('Origin',(0.0866025403784439,-0.4,0.15));
#6141=CARTESIAN_POINT('',(0.0866025403784439,-0.4,0.15));
#6142=CARTESIAN_POINT('',(-0.0866025403784439,-0.4,0.15));
#6143=CARTESIAN_POINT('',(0.0866025403784439,-0.64,0.15));
#6144=CARTESIAN_POINT('',(0.0866025403784439,-0.4,0.15));
#6145=CARTESIAN_POINT('',(-0.0866025403784439,-0.64,0.15));
#6146=CARTESIAN_POINT('Origin',(0.173205080756888,-0.4,0.));
#6147=CARTESIAN_POINT('',(0.0866025403784439,-0.4,0.15));
#6148=CARTESIAN_POINT('',(0.0866025403784439,-0.64,0.15));
#6149=CARTESIAN_POINT('Origin',(0.,-0.4,-2.77555756156289E-17));
#6150=CARTESIAN_POINT('Origin',(0.,-0.64,-2.77555756156289E-17));
#6151=CARTESIAN_POINT('',(0.,0.,0.));
#6152=CARTESIAN_POINT('',(0.,0.,0.));
#6153=CARTESIAN_POINT('',(0.,0.,0.));
#6154=CARTESIAN_POINT('',(0.,0.,0.));
#6155=CARTESIAN_POINT('',(0.,0.,0.));
#6156=CARTESIAN_POINT('',(0.,0.,0.));
#6157=CARTESIAN_POINT('',(0.,0.,0.));
#6158=CARTESIAN_POINT('',(0.,37.,0.));
#6159=CARTESIAN_POINT('',(-2.9,-2.,1.8));
#6160=CARTESIAN_POINT('',(-2.9,-2.,1.96));
#6161=CARTESIAN_POINT('',(2.9,-2.,1.8));
#6162=CARTESIAN_POINT('',(2.9,-2.,1.96));
#6163=CARTESIAN_POINT('',(-2.9,32.,1.8));
#6164=CARTESIAN_POINT('',(-2.9,32.,1.96));
#6165=CARTESIAN_POINT('',(2.9,32.,1.8));
#6166=CARTESIAN_POINT('',(2.9,32.,1.96));
#6167=CARTESIAN_POINT('',(0.,0.,0.));
#6168=CARTESIAN_POINT('',(0.,35.3,0.));
#6169=CARTESIAN_POINT('',(0.,-2.8,4.5));
#6170=CARTESIAN_POINT('',(0.,32.8,4.5));
#6171=CARTESIAN_POINT('',(0.,0.,0.));
#6172=CARTESIAN_POINT('',(0.,34.9,0.));
#6173=CARTESIAN_POINT('',(0.,0.45,4.5));
#6174=CARTESIAN_POINT('',(0.,29.55,4.5));
#6175=CARTESIAN_POINT('',(0.,0.,0.));
#6176=CARTESIAN_POINT('',(0.,0.,0.));
#6177=CARTESIAN_POINT('',(0.,0.,0.));
#6178=CARTESIAN_POINT('',(0.,0.,0.));
#6179=CARTESIAN_POINT('',(1.9,-0.3,4.5));
#6180=CARTESIAN_POINT('',(1.16341445918999E-16,-0.3,6.4));
#6181=CARTESIAN_POINT('',(-1.9,-0.3,4.5));
#6182=CARTESIAN_POINT('',(-3.49024337756996E-16,-0.3,2.6));
#6183=CARTESIAN_POINT('',(0.,30.3,0.));
#6184=CARTESIAN_POINT('',(1.9,30.3,4.5));
#6185=CARTESIAN_POINT('',(1.16341445919E-16,30.3,6.4));
#6186=CARTESIAN_POINT('',(-1.9,30.3,4.5));
#6187=CARTESIAN_POINT('',(-3.49024337756995E-16,30.3,2.6));
#6188=CARTESIAN_POINT('',(0.,0.,0.));
#6189=CARTESIAN_POINT('',(0.,0.,0.));
#6190=UNCERTAINTY_MEASURE_WITH_UNIT(LENGTH_MEASURE(0.001),#6242,
'DISTANCE_ACCURACY_VALUE',
'Maximum model space distance between geometric entities at asserted c
onnectivities');
#6191=UNCERTAINTY_MEASURE_WITH_UNIT(LENGTH_MEASURE(0.001),#6242,
'DISTANCE_ACCURACY_VALUE',
'Maximum model space distance between geometric entities at asserted c
onnectivities');
#6192=UNCERTAINTY_MEASURE_WITH_UNIT(LENGTH_MEASURE(0.001),#6242,
'DISTANCE_ACCURACY_VALUE',
'Maximum model space distance between geometric entities at asserted c
onnectivities');
#6193=UNCERTAINTY_MEASURE_WITH_UNIT(LENGTH_MEASURE(0.001),#6242,
'DISTANCE_ACCURACY_VALUE',
'Maximum model space distance between geometric entities at asserted c
onnectivities');
#6194=UNCERTAINTY_MEASURE_WITH_UNIT(LENGTH_MEASURE(0.001),#6242,
'DISTANCE_ACCURACY_VALUE',
'Maximum model space distance between geometric entities at asserted c
onnectivities');
#6195=UNCERTAINTY_MEASURE_WITH_UNIT(LENGTH_MEASURE(0.001),#6242,
'DISTANCE_ACCURACY_VALUE',
'Maximum model space distance between geometric entities at asserted c
onnectivities');
#6196=UNCERTAINTY_MEASURE_WITH_UNIT(LENGTH_MEASURE(0.001),#6242,
'DISTANCE_ACCURACY_VALUE',
'Maximum model space distance between geometric entities at asserted c
onnectivities');
#6197=UNCERTAINTY_MEASURE_WITH_UNIT(LENGTH_MEASURE(0.001),#6242,
'DISTANCE_ACCURACY_VALUE',
'Maximum model space distance between geometric entities at asserted c
onnectivities');
#6198=UNCERTAINTY_MEASURE_WITH_UNIT(LENGTH_MEASURE(0.001),#6242,
'DISTANCE_ACCURACY_VALUE',
'Maximum model space distance between geometric entities at asserted c
onnectivities');
#6199=UNCERTAINTY_MEASURE_WITH_UNIT(LENGTH_MEASURE(0.001),#6242,
'DISTANCE_ACCURACY_VALUE',
'Maximum model space distance between geometric entities at asserted c
onnectivities');
#6200=UNCERTAINTY_MEASURE_WITH_UNIT(LENGTH_MEASURE(0.001),#6242,
'DISTANCE_ACCURACY_VALUE',
'Maximum model space distance between geometric entities at asserted c
onnectivities');
#6201=UNCERTAINTY_MEASURE_WITH_UNIT(LENGTH_MEASURE(0.001),#6242,
'DISTANCE_ACCURACY_VALUE',
'Maximum model space distance between geometric entities at asserted c
onnectivities');
#6202=UNCERTAINTY_MEASURE_WITH_UNIT(LENGTH_MEASURE(0.001),#6242,
'DISTANCE_ACCURACY_VALUE',
'Maximum model space distance between geometric entities at asserted c
onnectivities');
#6203=UNCERTAINTY_MEASURE_WITH_UNIT(LENGTH_MEASURE(0.001),#6242,
'DISTANCE_ACCURACY_VALUE',
'Maximum model space distance between geometric entities at asserted c
onnectivities');
#6204=UNCERTAINTY_MEASURE_WITH_UNIT(LENGTH_MEASURE(0.001),#6242,
'DISTANCE_ACCURACY_VALUE',
'Maximum model space distance between geometric entities at asserted c
onnectivities');
#6205=UNCERTAINTY_MEASURE_WITH_UNIT(LENGTH_MEASURE(0.001),#6242,
'DISTANCE_ACCURACY_VALUE',
'Maximum model space distance between geometric entities at asserted c
onnectivities');
#6206=UNCERTAINTY_MEASURE_WITH_UNIT(LENGTH_MEASURE(0.001),#6242,
'DISTANCE_ACCURACY_VALUE',
'Maximum model space distance between geometric entities at asserted c
onnectivities');
#6207=UNCERTAINTY_MEASURE_WITH_UNIT(LENGTH_MEASURE(0.001),#6242,
'DISTANCE_ACCURACY_VALUE',
'Maximum model space distance between geometric entities at asserted c
onnectivities');
#6208=UNCERTAINTY_MEASURE_WITH_UNIT(LENGTH_MEASURE(0.001),#6242,
'DISTANCE_ACCURACY_VALUE',
'Maximum model space distance between geometric entities at asserted c
onnectivities');
#6209=UNCERTAINTY_MEASURE_WITH_UNIT(LENGTH_MEASURE(0.001),#6242,
'DISTANCE_ACCURACY_VALUE',
'Maximum model space distance between geometric entities at asserted c
onnectivities');
#6210=UNCERTAINTY_MEASURE_WITH_UNIT(LENGTH_MEASURE(0.001),#6242,
'DISTANCE_ACCURACY_VALUE',
'Maximum model space distance between geometric entities at asserted c
onnectivities');
#6211=UNCERTAINTY_MEASURE_WITH_UNIT(LENGTH_MEASURE(0.001),#6242,
'DISTANCE_ACCURACY_VALUE',
'Maximum model space distance between geometric entities at asserted c
onnectivities');
#6212=UNCERTAINTY_MEASURE_WITH_UNIT(LENGTH_MEASURE(0.001),#6242,
'DISTANCE_ACCURACY_VALUE',
'Maximum model space distance between geometric entities at asserted c
onnectivities');
#6213=UNCERTAINTY_MEASURE_WITH_UNIT(LENGTH_MEASURE(0.001),#6242,
'DISTANCE_ACCURACY_VALUE',
'Maximum model space distance between geometric entities at asserted c
onnectivities');
#6214=UNCERTAINTY_MEASURE_WITH_UNIT(LENGTH_MEASURE(0.001),#6242,
'DISTANCE_ACCURACY_VALUE',
'Maximum model space distance between geometric entities at asserted c
onnectivities');
#6215=UNCERTAINTY_MEASURE_WITH_UNIT(LENGTH_MEASURE(0.001),#6242,
'DISTANCE_ACCURACY_VALUE',
'Maximum model space distance between geometric entities at asserted c
onnectivities');
#6216=(
GEOMETRIC_REPRESENTATION_CONTEXT(3)
GLOBAL_UNCERTAINTY_ASSIGNED_CONTEXT((#6190))
GLOBAL_UNIT_ASSIGNED_CONTEXT((#6242,#6244,#6245))
REPRESENTATION_CONTEXT('','3D')
);
#6217=(
GEOMETRIC_REPRESENTATION_CONTEXT(3)
GLOBAL_UNCERTAINTY_ASSIGNED_CONTEXT((#6191))
GLOBAL_UNIT_ASSIGNED_CONTEXT((#6242,#6244,#6245))
REPRESENTATION_CONTEXT('','3D')
);
#6218=(
GEOMETRIC_REPRESENTATION_CONTEXT(3)
GLOBAL_UNCERTAINTY_ASSIGNED_CONTEXT((#6192))
GLOBAL_UNIT_ASSIGNED_CONTEXT((#6242,#6244,#6245))
REPRESENTATION_CONTEXT('','3D')
);
#6219=(
GEOMETRIC_REPRESENTATION_CONTEXT(3)
GLOBAL_UNCERTAINTY_ASSIGNED_CONTEXT((#6193))
GLOBAL_UNIT_ASSIGNED_CONTEXT((#6242,#6244,#6245))
REPRESENTATION_CONTEXT('','3D')
);
#6220=(
GEOMETRIC_REPRESENTATION_CONTEXT(3)
GLOBAL_UNCERTAINTY_ASSIGNED_CONTEXT((#6194))
GLOBAL_UNIT_ASSIGNED_CONTEXT((#6242,#6244,#6245))
REPRESENTATION_CONTEXT('','3D')
);
#6221=(
GEOMETRIC_REPRESENTATION_CONTEXT(3)
GLOBAL_UNCERTAINTY_ASSIGNED_CONTEXT((#6195))
GLOBAL_UNIT_ASSIGNED_CONTEXT((#6242,#6244,#6245))
REPRESENTATION_CONTEXT('','3D')
);
#6222=(
GEOMETRIC_REPRESENTATION_CONTEXT(3)
GLOBAL_UNCERTAINTY_ASSIGNED_CONTEXT((#6196))
GLOBAL_UNIT_ASSIGNED_CONTEXT((#6242,#6244,#6245))
REPRESENTATION_CONTEXT('','3D')
);
#6223=(
GEOMETRIC_REPRESENTATION_CONTEXT(3)
GLOBAL_UNCERTAINTY_ASSIGNED_CONTEXT((#6197))
GLOBAL_UNIT_ASSIGNED_CONTEXT((#6242,#6244,#6245))
REPRESENTATION_CONTEXT('','3D')
);
#6224=(
GEOMETRIC_REPRESENTATION_CONTEXT(3)
GLOBAL_UNCERTAINTY_ASSIGNED_CONTEXT((#6198))
GLOBAL_UNIT_ASSIGNED_CONTEXT((#6242,#6244,#6245))
REPRESENTATION_CONTEXT('','3D')
);
#6225=(
GEOMETRIC_REPRESENTATION_CONTEXT(3)
GLOBAL_UNCERTAINTY_ASSIGNED_CONTEXT((#6199))
GLOBAL_UNIT_ASSIGNED_CONTEXT((#6242,#6244,#6245))
REPRESENTATION_CONTEXT('','3D')
);
#6226=(
GEOMETRIC_REPRESENTATION_CONTEXT(3)
GLOBAL_UNCERTAINTY_ASSIGNED_CONTEXT((#6200))
GLOBAL_UNIT_ASSIGNED_CONTEXT((#6242,#6244,#6245))
REPRESENTATION_CONTEXT('','3D')
);
#6227=(
GEOMETRIC_REPRESENTATION_CONTEXT(3)
GLOBAL_UNCERTAINTY_ASSIGNED_CONTEXT((#6201))
GLOBAL_UNIT_ASSIGNED_CONTEXT((#6242,#6244,#6245))
REPRESENTATION_CONTEXT('','3D')
);
#6228=(
GEOMETRIC_REPRESENTATION_CONTEXT(3)
GLOBAL_UNCERTAINTY_ASSIGNED_CONTEXT((#6202))
GLOBAL_UNIT_ASSIGNED_CONTEXT((#6242,#6244,#6245))
REPRESENTATION_CONTEXT('','3D')
);
#6229=(
GEOMETRIC_REPRESENTATION_CONTEXT(3)
GLOBAL_UNCERTAINTY_ASSIGNED_CONTEXT((#6203))
GLOBAL_UNIT_ASSIGNED_CONTEXT((#6242,#6244,#6245))
REPRESENTATION_CONTEXT('','3D')
);
#6230=(
GEOMETRIC_REPRESENTATION_CONTEXT(3)
GLOBAL_UNCERTAINTY_ASSIGNED_CONTEXT((#6204))
GLOBAL_UNIT_ASSIGNED_CONTEXT((#6242,#6244,#6245))
REPRESENTATION_CONTEXT('','3D')
);
#6231=(
GEOMETRIC_REPRESENTATION_CONTEXT(3)
GLOBAL_UNCERTAINTY_ASSIGNED_CONTEXT((#6205))
GLOBAL_UNIT_ASSIGNED_CONTEXT((#6242,#6244,#6245))
REPRESENTATION_CONTEXT('','3D')
);
#6232=(
GEOMETRIC_REPRESENTATION_CONTEXT(3)
GLOBAL_UNCERTAINTY_ASSIGNED_CONTEXT((#6206))
GLOBAL_UNIT_ASSIGNED_CONTEXT((#6242,#6244,#6245))
REPRESENTATION_CONTEXT('','3D')
);
#6233=(
GEOMETRIC_REPRESENTATION_CONTEXT(3)
GLOBAL_UNCERTAINTY_ASSIGNED_CONTEXT((#6207))
GLOBAL_UNIT_ASSIGNED_CONTEXT((#6242,#6244,#6245))
REPRESENTATION_CONTEXT('','3D')
);
#6234=(
GEOMETRIC_REPRESENTATION_CONTEXT(3)
GLOBAL_UNCERTAINTY_ASSIGNED_CONTEXT((#6208))
GLOBAL_UNIT_ASSIGNED_CONTEXT((#6242,#6244,#6245))
REPRESENTATION_CONTEXT('','3D')
);
#6235=(
GEOMETRIC_REPRESENTATION_CONTEXT(3)
GLOBAL_UNCERTAINTY_ASSIGNED_CONTEXT((#6209))
GLOBAL_UNIT_ASSIGNED_CONTEXT((#6242,#6244,#6245))
REPRESENTATION_CONTEXT('','3D')
);
#6236=(
GEOMETRIC_REPRESENTATION_CONTEXT(3)
GLOBAL_UNCERTAINTY_ASSIGNED_CONTEXT((#6210))
GLOBAL_UNIT_ASSIGNED_CONTEXT((#6242,#6244,#6245))
REPRESENTATION_CONTEXT('','3D')
);
#6237=(
GEOMETRIC_REPRESENTATION_CONTEXT(3)
GLOBAL_UNCERTAINTY_ASSIGNED_CONTEXT((#6211))
GLOBAL_UNIT_ASSIGNED_CONTEXT((#6242,#6244,#6245))
REPRESENTATION_CONTEXT('','3D')
);
#6238=(
GEOMETRIC_REPRESENTATION_CONTEXT(3)
GLOBAL_UNCERTAINTY_ASSIGNED_CONTEXT((#6212))
GLOBAL_UNIT_ASSIGNED_CONTEXT((#6242,#6244,#6245))
REPRESENTATION_CONTEXT('','3D')
);
#6239=(
GEOMETRIC_REPRESENTATION_CONTEXT(3)
GLOBAL_UNCERTAINTY_ASSIGNED_CONTEXT((#6213))
GLOBAL_UNIT_ASSIGNED_CONTEXT((#6242,#6244,#6245))
REPRESENTATION_CONTEXT('','3D')
);
#6240=(
GEOMETRIC_REPRESENTATION_CONTEXT(3)
GLOBAL_UNCERTAINTY_ASSIGNED_CONTEXT((#6214))
GLOBAL_UNIT_ASSIGNED_CONTEXT((#6242,#6244,#6245))
REPRESENTATION_CONTEXT('','3D')
);
#6241=(
GEOMETRIC_REPRESENTATION_CONTEXT(3)
GLOBAL_UNCERTAINTY_ASSIGNED_CONTEXT((#6215))
GLOBAL_UNIT_ASSIGNED_CONTEXT((#6242,#6244,#6245))
REPRESENTATION_CONTEXT('','3D')
);
#6242=(
LENGTH_UNIT()
NAMED_UNIT(*)
SI_UNIT(.CENTI.,.METRE.)
);
#6243=(
LENGTH_UNIT()
NAMED_UNIT(*)
SI_UNIT($,.METRE.)
);
#6244=(
NAMED_UNIT(*)
PLANE_ANGLE_UNIT()
SI_UNIT($,.RADIAN.)
);
#6245=(
NAMED_UNIT(*)
SI_UNIT($,.STERADIAN.)
SOLID_ANGLE_UNIT()
);
#6246=SHAPE_DEFINITION_REPRESENTATION(#6271,#6340);
#6247=SHAPE_DEFINITION_REPRESENTATION(#6272,#6341);
#6248=SHAPE_DEFINITION_REPRESENTATION(#6273,#6342);
#6249=SHAPE_DEFINITION_REPRESENTATION(#6274,#6343);
#6250=SHAPE_DEFINITION_REPRESENTATION(#6275,#6344);
#6251=SHAPE_DEFINITION_REPRESENTATION(#6276,#6345);
#6252=SHAPE_DEFINITION_REPRESENTATION(#6277,#6346);
#6253=SHAPE_DEFINITION_REPRESENTATION(#6278,#6347);
#6254=SHAPE_DEFINITION_REPRESENTATION(#6279,#6348);
#6255=SHAPE_DEFINITION_REPRESENTATION(#6280,#6349);
#6256=SHAPE_DEFINITION_REPRESENTATION(#6281,#6350);
#6257=SHAPE_DEFINITION_REPRESENTATION(#6282,#6351);
#6258=SHAPE_DEFINITION_REPRESENTATION(#6283,#6352);
#6259=SHAPE_DEFINITION_REPRESENTATION(#6284,#6353);
#6260=SHAPE_DEFINITION_REPRESENTATION(#6285,#6354);
#6261=SHAPE_DEFINITION_REPRESENTATION(#6286,#6355);
#6262=SHAPE_DEFINITION_REPRESENTATION(#6287,#6356);
#6263=SHAPE_DEFINITION_REPRESENTATION(#6288,#6357);
#6264=SHAPE_DEFINITION_REPRESENTATION(#6289,#6358);
#6265=SHAPE_DEFINITION_REPRESENTATION(#6295,#6359);
#6266=SHAPE_DEFINITION_REPRESENTATION(#6296,#6360);
#6267=SHAPE_DEFINITION_REPRESENTATION(#6297,#6361);
#6268=SHAPE_DEFINITION_REPRESENTATION(#6298,#6362);
#6269=SHAPE_DEFINITION_REPRESENTATION(#6299,#6363);
#6270=SHAPE_DEFINITION_REPRESENTATION(#6300,#6364);
#6271=PRODUCT_DEFINITION_SHAPE('',$,#6366);
#6272=PRODUCT_DEFINITION_SHAPE('',$,#6367);
#6273=PRODUCT_DEFINITION_SHAPE('',$,#6368);
#6274=PRODUCT_DEFINITION_SHAPE('',$,#6369);
#6275=PRODUCT_DEFINITION_SHAPE('',$,#6370);
#6276=PRODUCT_DEFINITION_SHAPE('',$,#6371);
#6277=PRODUCT_DEFINITION_SHAPE('',$,#6372);
#6278=PRODUCT_DEFINITION_SHAPE('',$,#6373);
#6279=PRODUCT_DEFINITION_SHAPE('',$,#6374);
#6280=PRODUCT_DEFINITION_SHAPE('',$,#6375);
#6281=PRODUCT_DEFINITION_SHAPE('',$,#6376);
#6282=PRODUCT_DEFINITION_SHAPE('',$,#6377);
#6283=PRODUCT_DEFINITION_SHAPE('',$,#6378);
#6284=PRODUCT_DEFINITION_SHAPE('',$,#6379);
#6285=PRODUCT_DEFINITION_SHAPE('',$,#6380);
#6286=PRODUCT_DEFINITION_SHAPE('',$,#6381);
#6287=PRODUCT_DEFINITION_SHAPE('',$,#6382);
#6288=PRODUCT_DEFINITION_SHAPE('',$,#6383);
#6289=PRODUCT_DEFINITION_SHAPE('',$,#6384);
#6290=PRODUCT_DEFINITION_SHAPE($,$,#143);
#6291=PRODUCT_DEFINITION_SHAPE($,$,#144);
#6292=PRODUCT_DEFINITION_SHAPE($,$,#145);
#6293=PRODUCT_DEFINITION_SHAPE($,$,#146);
#6294=PRODUCT_DEFINITION_SHAPE($,$,#147);
#6295=PRODUCT_DEFINITION_SHAPE('',$,#6385);
#6296=PRODUCT_DEFINITION_SHAPE('',$,#6386);
#6297=PRODUCT_DEFINITION_SHAPE('',$,#6387);
#6298=PRODUCT_DEFINITION_SHAPE('',$,#6388);
#6299=PRODUCT_DEFINITION_SHAPE('',$,#6389);
#6300=PRODUCT_DEFINITION_SHAPE('',$,#6390);
#6301=PRODUCT_DEFINITION_SHAPE($,$,#148);
#6302=PRODUCT_DEFINITION_SHAPE($,$,#149);
#6303=PRODUCT_DEFINITION_SHAPE($,$,#150);
#6304=PRODUCT_DEFINITION_SHAPE($,$,#151);
#6305=PRODUCT_DEFINITION_SHAPE($,$,#152);
#6306=PRODUCT_DEFINITION_SHAPE($,$,#153);
#6307=PRODUCT_DEFINITION_SHAPE($,$,#154);
#6308=PRODUCT_DEFINITION_SHAPE($,$,#155);
#6309=PRODUCT_DEFINITION_SHAPE($,$,#156);
#6310=PRODUCT_DEFINITION_SHAPE($,$,#157);
#6311=PRODUCT_DEFINITION_SHAPE($,$,#158);
#6312=PRODUCT_DEFINITION_SHAPE($,$,#159);
#6313=PRODUCT_DEFINITION_SHAPE($,$,#160);
#6314=PRODUCT_DEFINITION_SHAPE($,$,#161);
#6315=PRODUCT_DEFINITION_SHAPE($,$,#162);
#6316=PRODUCT_DEFINITION_SHAPE($,$,#163);
#6317=PRODUCT_DEFINITION_SHAPE($,$,#164);
#6318=PRODUCT_DEFINITION_SHAPE($,$,#165);
#6319=PRODUCT_DEFINITION_SHAPE($,$,#166);
#6320=PRODUCT_DEFINITION_SHAPE($,$,#167);
#6321=PRODUCT_DEFINITION_SHAPE($,$,#168);
#6322=PRODUCT_DEFINITION_SHAPE($,$,#169);
#6323=PRODUCT_DEFINITION_SHAPE($,$,#170);
#6324=PRODUCT_DEFINITION_SHAPE($,$,#171);
#6325=PRODUCT_DEFINITION_SHAPE($,$,#172);
#6326=PRODUCT_DEFINITION_SHAPE($,$,#173);
#6327=PRODUCT_DEFINITION_SHAPE($,$,#174);
#6328=PRODUCT_DEFINITION_SHAPE($,$,#175);
#6329=PRODUCT_DEFINITION_SHAPE($,$,#176);
#6330=PRODUCT_DEFINITION_SHAPE($,$,#177);
#6331=PRODUCT_DEFINITION_SHAPE($,$,#178);
#6332=PRODUCT_DEFINITION_SHAPE($,$,#179);
#6333=PRODUCT_DEFINITION_SHAPE($,$,#180);
#6334=PRODUCT_DEFINITION_SHAPE($,$,#181);
#6335=PRODUCT_DEFINITION_SHAPE($,$,#182);
#6336=PRODUCT_DEFINITION_SHAPE($,$,#183);
#6337=PRODUCT_DEFINITION_SHAPE($,$,#184);
#6338=PRODUCT_DEFINITION_SHAPE($,$,#185);
#6339=PRODUCT_DEFINITION_SHAPE($,$,#186);
#6340=SHAPE_REPRESENTATION('',(#3445,#3884,#3885),#6216);
#6341=SHAPE_REPRESENTATION('',(#3446,#3847,#3848,#3849,#3850,#3851,#3852,
#3853,#3854,#3855,#3856,#3857,#3858,#3859,#3860,#3861,#3862,#3863,#3864,
#3865,#3866,#3867,#3868,#3869,#3870),#6217);
#6342=SHAPE_REPRESENTATION('',(#3447),#6218);
#6343=SHAPE_REPRESENTATION('',(#3468),#6219);
#6344=SHAPE_REPRESENTATION('',(#3489),#6220);
#6345=SHAPE_REPRESENTATION('',(#3511),#6221);
#6346=SHAPE_REPRESENTATION('',(#3520),#6222);
#6347=SHAPE_REPRESENTATION('',(#3529),#6223);
#6348=SHAPE_REPRESENTATION('',(#3548),#6224);
#6349=SHAPE_REPRESENTATION('',(#3555),#6225);
#6350=SHAPE_REPRESENTATION('',(#3564),#6226);
#6351=SHAPE_REPRESENTATION('',(#3588),#6227);
#6352=SHAPE_REPRESENTATION('',(#3597),#6228);
#6353=SHAPE_REPRESENTATION('',(#3606,#3735,#3736,#3737,#3738,#3739),#6229);
#6354=SHAPE_REPRESENTATION('',(#3607),#6230);
#6355=SHAPE_REPRESENTATION('',(#3627),#6231);
#6356=SHAPE_REPRESENTATION('',(#3647),#6232);
#6357=SHAPE_REPRESENTATION('',(#3664),#6233);
#6358=SHAPE_REPRESENTATION('',(#3718),#6234);
#6359=SHAPE_REPRESENTATION('',(#3740,#3871,#3872,#3873,#3874,#3875,#3876,
#3877,#3878,#3879,#3880,#3881,#3882,#3883),#6235);
#6360=SHAPE_REPRESENTATION('',(#3741),#6236);
#6361=SHAPE_REPRESENTATION('',(#3766),#6237);
#6362=SHAPE_REPRESENTATION('',(#3791),#6238);
#6363=SHAPE_REPRESENTATION('',(#3800),#6239);
#6364=SHAPE_REPRESENTATION('',(#3821),#6240);
#6365=PRODUCT_DEFINITION_CONTEXT('part definition',#6442,'design');
#6366=PRODUCT_DEFINITION('PAT-016','PAT-016',#6391,
#6365);
#6367=PRODUCT_DEFINITION('Axle brackets and bearings',
'Axle brackets and bearings',#6392,#6365);
#6368=PRODUCT_DEFINITION('Axle bracket','Axle bracket',#6393,#6365);
#6369=PRODUCT_DEFINITION('Axle bracket (1)','Axle bracket (1)',#6394,#6365);
#6370=PRODUCT_DEFINITION('Stepped axle','Stepped axle',#6395,#6365);
#6371=PRODUCT_DEFINITION('Journal spacer','Journal spacer',#6396,#6365);
#6372=PRODUCT_DEFINITION('Journal spacer (1)','Journal spacer (1)',#6397,
#6365);
#6373=PRODUCT_DEFINITION('Base','Base',#6398,#6365);
#6374=PRODUCT_DEFINITION('Bonded foot pad','Bonded foot pad',#6399,#6365);
#6375=PRODUCT_DEFINITION('Flat Washer - M6','Flat Washer - M6',#6400,#6365);
#6376=PRODUCT_DEFINITION('M6x18 mounting screw','M6x18 mounting screw',
#6401,#6365);
#6377=PRODUCT_DEFINITION('End keeper','End keeper',#6402,#6365);
#6378=PRODUCT_DEFINITION('Bracket shim','Bracket shim',#6403,#6365);
#6379=PRODUCT_DEFINITION('Cleared radial bearing',
'Cleared radial bearing',#6404,#6365);
#6380=PRODUCT_DEFINITION('Inner ring','Inner ring',#6405,#6365);
#6381=PRODUCT_DEFINITION('Outer ring','Outer ring',#6406,#6365);
#6382=PRODUCT_DEFINITION('Balls','Balls',#6407,#6365);
#6383=PRODUCT_DEFINITION('Cage','Cage',#6408,#6365);
#6384=PRODUCT_DEFINITION('Seals 2RS','Seals 2RS',#6409,#6365);
#6385=PRODUCT_DEFINITION('Roller tube and end caps',
'Roller tube and end caps',#6410,#6365);
#6386=PRODUCT_DEFINITION('Bearing insert','Bearing insert',#6411,#6365);
#6387=PRODUCT_DEFINITION('Bearing insert (1)','Bearing insert (1)',#6412,
#6365);
#6388=PRODUCT_DEFINITION('Roller tube','Roller tube',#6413,#6365);
#6389=PRODUCT_DEFINITION('Outer race retainer','Outer race retainer',#6414,
#6365);
#6390=PRODUCT_DEFINITION('Cap Screw - M4x16','Cap Screw - M4x16',#6415,
#6365);
#6391=PRODUCT_DEFINITION_FORMATION('',$,#6444);
#6392=PRODUCT_DEFINITION_FORMATION('',$,#6445);
#6393=PRODUCT_DEFINITION_FORMATION('',$,#6446);
#6394=PRODUCT_DEFINITION_FORMATION('',$,#6447);
#6395=PRODUCT_DEFINITION_FORMATION('',$,#6448);
#6396=PRODUCT_DEFINITION_FORMATION('',$,#6449);
#6397=PRODUCT_DEFINITION_FORMATION('',$,#6450);
#6398=PRODUCT_DEFINITION_FORMATION('',$,#6451);
#6399=PRODUCT_DEFINITION_FORMATION('',$,#6452);
#6400=PRODUCT_DEFINITION_FORMATION('',$,#6453);
#6401=PRODUCT_DEFINITION_FORMATION('',$,#6454);
#6402=PRODUCT_DEFINITION_FORMATION('',$,#6455);
#6403=PRODUCT_DEFINITION_FORMATION('',$,#6456);
#6404=PRODUCT_DEFINITION_FORMATION('',$,#6457);
#6405=PRODUCT_DEFINITION_FORMATION('',$,#6458);
#6406=PRODUCT_DEFINITION_FORMATION('',$,#6459);
#6407=PRODUCT_DEFINITION_FORMATION('',$,#6460);
#6408=PRODUCT_DEFINITION_FORMATION('',$,#6461);
#6409=PRODUCT_DEFINITION_FORMATION('',$,#6462);
#6410=PRODUCT_DEFINITION_FORMATION('',$,#6463);
#6411=PRODUCT_DEFINITION_FORMATION('',$,#6464);
#6412=PRODUCT_DEFINITION_FORMATION('',$,#6465);
#6413=PRODUCT_DEFINITION_FORMATION('',$,#6466);
#6414=PRODUCT_DEFINITION_FORMATION('',$,#6467);
#6415=PRODUCT_DEFINITION_FORMATION('',$,#6468);
#6416=PRODUCT_RELATED_PRODUCT_CATEGORY('PAT-016','PAT-016',(#6444));
#6417=PRODUCT_RELATED_PRODUCT_CATEGORY('Axle brackets and bearings',
'Axle brackets and bearings',(#6445));
#6418=PRODUCT_RELATED_PRODUCT_CATEGORY('Axle bracket','Axle bracket',(#6446));
#6419=PRODUCT_RELATED_PRODUCT_CATEGORY('Axle bracket (1)',
'Axle bracket (1)',(#6447));
#6420=PRODUCT_RELATED_PRODUCT_CATEGORY('Stepped axle','Stepped axle',(#6448));
#6421=PRODUCT_RELATED_PRODUCT_CATEGORY('Journal spacer',
'Journal spacer',(#6449));
#6422=PRODUCT_RELATED_PRODUCT_CATEGORY('Journal spacer (1)',
'Journal spacer (1)',(#6450));
#6423=PRODUCT_RELATED_PRODUCT_CATEGORY('Base','Base',(#6451));
#6424=PRODUCT_RELATED_PRODUCT_CATEGORY('Bonded foot pad',
'Bonded foot pad',(#6452));
#6425=PRODUCT_RELATED_PRODUCT_CATEGORY('Flat Washer - M6',
'Flat Washer - M6',(#6453));
#6426=PRODUCT_RELATED_PRODUCT_CATEGORY('M6x18 mounting screw',
'M6x18 mounting screw',(#6454));
#6427=PRODUCT_RELATED_PRODUCT_CATEGORY('End keeper','End keeper',(#6455));
#6428=PRODUCT_RELATED_PRODUCT_CATEGORY('Bracket shim','Bracket shim',(#6456));
#6429=PRODUCT_RELATED_PRODUCT_CATEGORY('Cleared radial bearing',
'Cleared radial bearing',(#6457));
#6430=PRODUCT_RELATED_PRODUCT_CATEGORY('Inner ring','Inner ring',(#6458));
#6431=PRODUCT_RELATED_PRODUCT_CATEGORY('Outer ring','Outer ring',(#6459));
#6432=PRODUCT_RELATED_PRODUCT_CATEGORY('Balls','Balls',(#6460));
#6433=PRODUCT_RELATED_PRODUCT_CATEGORY('Cage','Cage',(#6461));
#6434=PRODUCT_RELATED_PRODUCT_CATEGORY('Seals 2RS','Seals 2RS',(#6462));
#6435=PRODUCT_RELATED_PRODUCT_CATEGORY('Roller tube and end caps',
'Roller tube and end caps',(#6463));
#6436=PRODUCT_RELATED_PRODUCT_CATEGORY('Bearing insert',
'Bearing insert',(#6464));
#6437=PRODUCT_RELATED_PRODUCT_CATEGORY('Bearing insert (1)',
'Bearing insert (1)',(#6465));
#6438=PRODUCT_RELATED_PRODUCT_CATEGORY('Roller tube','Roller tube',(#6466));
#6439=PRODUCT_RELATED_PRODUCT_CATEGORY('Outer race retainer',
'Outer race retainer',(#6467));
#6440=PRODUCT_RELATED_PRODUCT_CATEGORY('Cap Screw - M4x16',
'Cap Screw - M4x16',(#6468));
#6441=APPLICATION_PROTOCOL_DEFINITION('international standard',
'automotive_design',2009,#6442);
#6442=APPLICATION_CONTEXT(
'Core Data for Automotive Mechanical Design Process');
#6443=PRODUCT_CONTEXT('part definition',#6442,'mechanical');
#6444=PRODUCT('PAT-016','PAT-016',
'PAT-016',(#6443));
#6445=PRODUCT('Axle brackets and bearings','Axle brackets and bearings',
'Axle brackets and bearings',(#6443));
#6446=PRODUCT('Axle bracket','Axle bracket','Axle bracket',(#6443));
#6447=PRODUCT('Axle bracket (1)','Axle bracket (1)','Axle bracket (1)',(#6443));
#6448=PRODUCT('Stepped axle','Stepped axle','Stepped axle',(#6443));
#6449=PRODUCT('Journal spacer','Journal spacer','Journal spacer',(#6443));
#6450=PRODUCT('Journal spacer (1)','Journal spacer (1)','Journal spacer (1)',
(#6443));
#6451=PRODUCT('Base','Base','Base',(#6443));
#6452=PRODUCT('Bonded foot pad','Bonded foot pad','Bonded foot pad',(#6443));
#6453=PRODUCT('Flat Washer - M6','Flat Washer - M6','Flat Washer - M6',
(#6443));
#6454=PRODUCT('M6x18 mounting screw','M6x18 mounting screw',
'M6x18 mounting screw',(#6443));
#6455=PRODUCT('End keeper','End keeper','End keeper',(#6443));
#6456=PRODUCT('Bracket shim','Bracket shim','Bracket shim',(#6443));
#6457=PRODUCT('Cleared radial bearing','Cleared radial bearing',
'Cleared radial bearing',(#6443));
#6458=PRODUCT('Inner ring','Inner ring','Inner ring',(#6443));
#6459=PRODUCT('Outer ring','Outer ring','Outer ring',(#6443));
#6460=PRODUCT('Balls','Balls','Balls',(#6443));
#6461=PRODUCT('Cage','Cage','Cage',(#6443));
#6462=PRODUCT('Seals 2RS','Seals 2RS','Seals 2RS',(#6443));
#6463=PRODUCT('Roller tube and end caps','Roller tube and end caps',
'Roller tube and end caps',(#6443));
#6464=PRODUCT('Bearing insert','Bearing insert','Bearing insert',(#6443));
#6465=PRODUCT('Bearing insert (1)','Bearing insert (1)','Bearing insert (1)',
(#6443));
#6466=PRODUCT('Roller tube','Roller tube','Roller tube',(#6443));
#6467=PRODUCT('Outer race retainer','Outer race retainer',
'Outer race retainer',(#6443));
#6468=PRODUCT('Cap Screw - M4x16','Cap Screw - M4x16',
'Cap Screw - M4x16',(#6443));
#6469=PRESENTATION_STYLE_ASSIGNMENT((#6475));
#6470=PRESENTATION_STYLE_ASSIGNMENT((#6476));
#6471=PRESENTATION_STYLE_ASSIGNMENT((#6477));
#6472=PRESENTATION_STYLE_ASSIGNMENT((#6478));
#6473=PRESENTATION_STYLE_ASSIGNMENT((#6479));
#6474=PRESENTATION_STYLE_ASSIGNMENT((#6480));
#6475=SURFACE_STYLE_USAGE(.BOTH.,#6481);
#6476=SURFACE_STYLE_USAGE(.BOTH.,#6482);
#6477=SURFACE_STYLE_USAGE(.BOTH.,#6483);
#6478=SURFACE_STYLE_USAGE(.BOTH.,#6484);
#6479=SURFACE_STYLE_USAGE(.BOTH.,#6485);
#6480=SURFACE_STYLE_USAGE(.BOTH.,#6486);
#6481=SURFACE_SIDE_STYLE('',(#6487));
#6482=SURFACE_SIDE_STYLE('',(#6488));
#6483=SURFACE_SIDE_STYLE('',(#6489));
#6484=SURFACE_SIDE_STYLE('',(#6490));
#6485=SURFACE_SIDE_STYLE('',(#6491));
#6486=SURFACE_SIDE_STYLE('',(#6492));
#6487=SURFACE_STYLE_FILL_AREA(#6493);
#6488=SURFACE_STYLE_FILL_AREA(#6494);
#6489=SURFACE_STYLE_FILL_AREA(#6495);
#6490=SURFACE_STYLE_FILL_AREA(#6496);
#6491=SURFACE_STYLE_FILL_AREA(#6497);
#6492=SURFACE_STYLE_FILL_AREA(#6498);
#6493=FILL_AREA_STYLE('Steel - Satin',(#6499));
#6494=FILL_AREA_STYLE('CAD Library Painted - Engineering blue',(#6500));
#6495=FILL_AREA_STYLE('CAD Library Painted - Steel gray',(#6501));
#6496=FILL_AREA_STYLE('CAD Library Painted - Deep blue',(#6502));
#6497=FILL_AREA_STYLE('CAD Library Painted - Graphite',(#6503));
#6498=FILL_AREA_STYLE('CAD Library Painted - Off white',(#6504));
#6499=FILL_AREA_STYLE_COLOUR('Steel - Satin',#6505);
#6500=FILL_AREA_STYLE_COLOUR('CAD Library Painted - Engineering blue',#6506);
#6501=FILL_AREA_STYLE_COLOUR('CAD Library Painted - Steel gray',#6507);
#6502=FILL_AREA_STYLE_COLOUR('CAD Library Painted - Deep blue',#6508);
#6503=FILL_AREA_STYLE_COLOUR('CAD Library Painted - Graphite',#6509);
#6504=FILL_AREA_STYLE_COLOUR('CAD Library Painted - Off white',#6510);
#6505=COLOUR_RGB('Steel - Satin',0.627450980392157,0.627450980392157,0.627450980392157);
#6506=COLOUR_RGB('CAD Library Painted - Engineering blue',0.12156862745098,
0.356862745098039,0.6);
#6507=COLOUR_RGB('CAD Library Painted - Steel gray',0.592156862745098,0.631372549019608,
0.67843137254902);
#6508=COLOUR_RGB('CAD Library Painted - Deep blue',0.0784313725490196,0.203921568627451,
0.349019607843137);
#6509=COLOUR_RGB('CAD Library Painted - Graphite',0.0980392156862745,0.109803921568627,
0.125490196078431);
#6510=COLOUR_RGB('CAD Library Painted - Off white',0.909803921568627,0.901960784313726,
0.858823529411765);
#6511=COLOUR_RGB('Dark Blue',0.08,0.2,0.34);
#6512=FILL_AREA_STYLE_COLOUR('',#6511);
#6513=FILL_AREA_STYLE('',(#6512));
#6514=SURFACE_STYLE_FILL_AREA(#6513);
#6515=SURFACE_SIDE_STYLE('',(#6514));
#6516=SURFACE_STYLE_USAGE(.BOTH.,#6515);
#6517=PRESENTATION_STYLE_ASSIGNMENT((#6516));
#6518=COLOUR_RGB('Light Blue',0.38,0.62,0.78);
#6519=FILL_AREA_STYLE_COLOUR('',#6518);
#6520=FILL_AREA_STYLE('',(#6519));
#6521=SURFACE_STYLE_FILL_AREA(#6520);
#6522=SURFACE_SIDE_STYLE('',(#6521));
#6523=SURFACE_STYLE_USAGE(.BOTH.,#6522);
#6524=PRESENTATION_STYLE_ASSIGNMENT((#6523));
#6525=COLOUR_RGB('Sky Blue',0.24,0.69,0.87);
#6526=FILL_AREA_STYLE_COLOUR('',#6525);
#6527=FILL_AREA_STYLE('',(#6526));
#6528=SURFACE_STYLE_FILL_AREA(#6527);
#6529=SURFACE_SIDE_STYLE('',(#6528));
#6530=SURFACE_STYLE_USAGE(.BOTH.,#6529);
#6531=PRESENTATION_STYLE_ASSIGNMENT((#6530));
#6532=COLOUR_RGB('Grey',0.48,0.52,0.57);
#6533=FILL_AREA_STYLE_COLOUR('',#6532);
#6534=FILL_AREA_STYLE('',(#6533));
#6535=SURFACE_STYLE_FILL_AREA(#6534);
#6536=SURFACE_SIDE_STYLE('',(#6535));
#6537=SURFACE_STYLE_USAGE(.BOTH.,#6536);
#6538=PRESENTATION_STYLE_ASSIGNMENT((#6537));
#6539=COLOUR_RGB('Black',0.12,0.14,0.17);
#6540=FILL_AREA_STYLE_COLOUR('',#6539);
#6541=FILL_AREA_STYLE('',(#6540));
#6542=SURFACE_STYLE_FILL_AREA(#6541);
#6543=SURFACE_SIDE_STYLE('',(#6542));
#6544=SURFACE_STYLE_USAGE(.BOTH.,#6543);
#6545=PRESENTATION_STYLE_ASSIGNMENT((#6544));
#6546=COLOUR_RGB('Off White',0.89,0.88,0.83);
#6547=FILL_AREA_STYLE_COLOUR('',#6546);
#6548=FILL_AREA_STYLE('',(#6547));
#6549=SURFACE_STYLE_FILL_AREA(#6548);
#6550=SURFACE_SIDE_STYLE('',(#6549));
#6551=SURFACE_STYLE_USAGE(.BOTH.,#6550);
#6552=PRESENTATION_STYLE_ASSIGNMENT((#6551));
ENDSEC;
END-ISO-10303-21;
